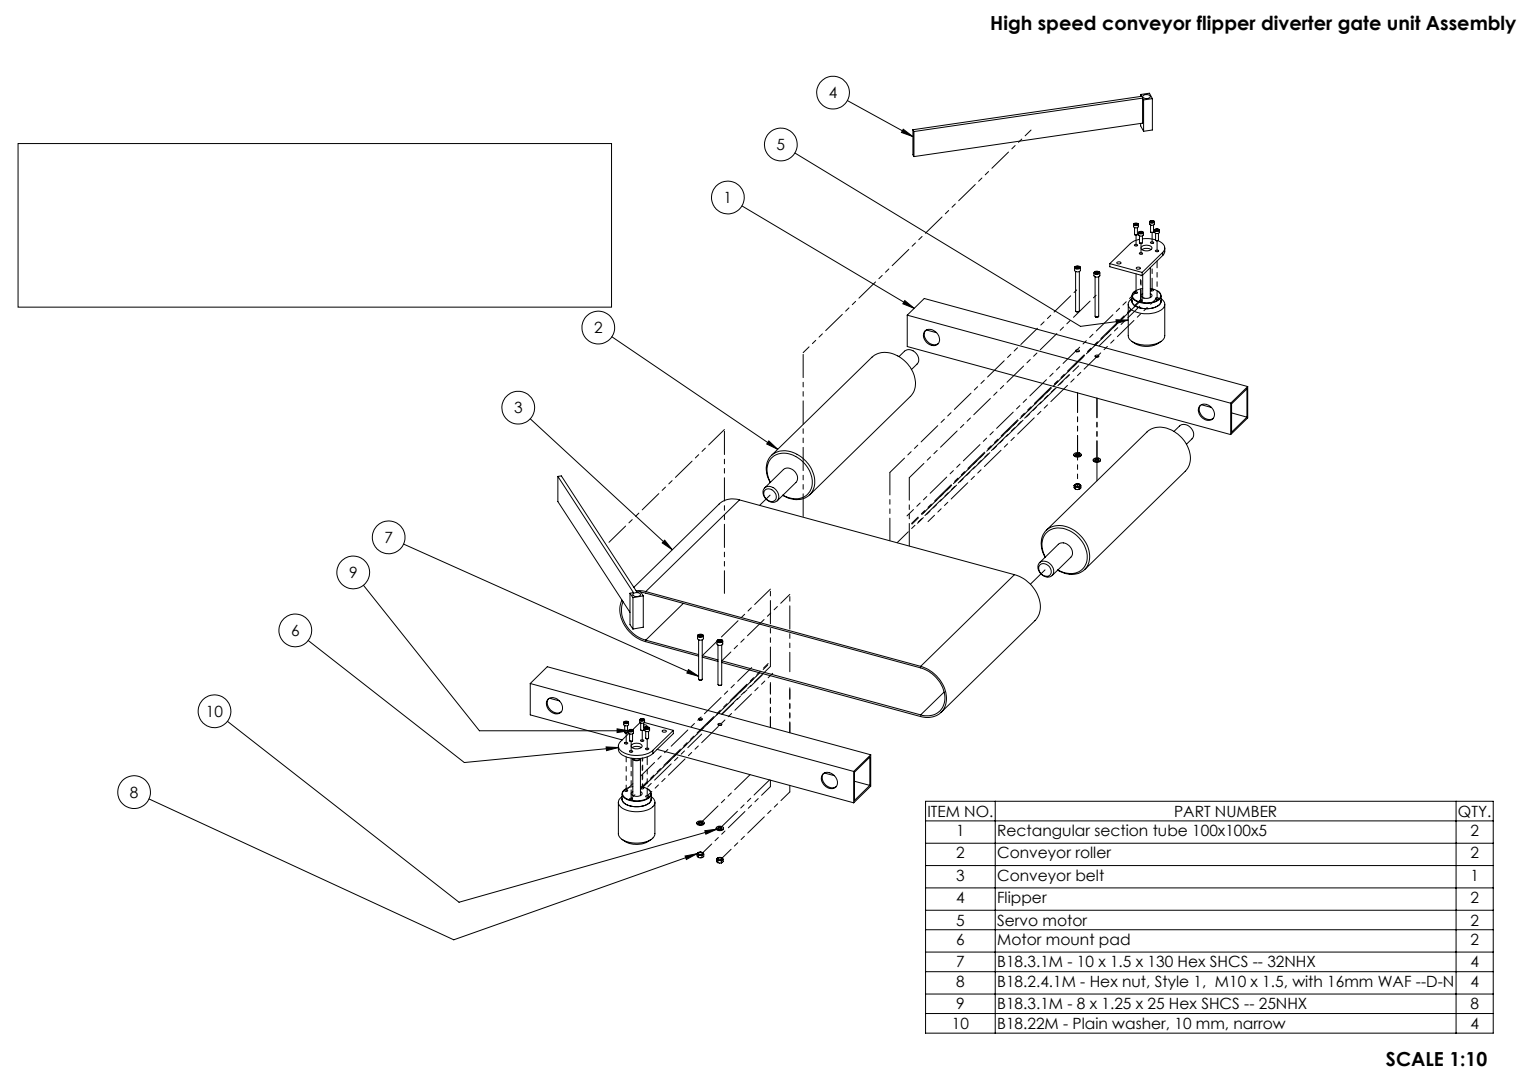
ISO-10303-21;
HEADER;
FILE_DESCRIPTION (('STEP AP214'),
    '1' );
FILE_NAME ('MAT-028',
    '2026-10-24T15:53:57',
    ( '' ),
    ( '' ),
    'SwSTEP 2.0',
    'SolidWorks 2025',
    '' );
FILE_SCHEMA (( 'AUTOMOTIVE_DESIGN' ));
ENDSEC;

DATA;
#1 = CARTESIAN_POINT ( 'NONE',  ( -86.99999999999945999, 120.0000000000003126, 10.00000000000000888 ) ) ;
#2 = DIRECTION ( 'NONE',  ( -3.851859888774471706E-33, -1.232595164407830946E-32, -1.000000000000000000 ) ) ;
#3 = FACE_BOUND ( 'NONE', #2659, .T. ) ;
#4 = FACE_BOUND ( 'NONE', #3829, .T. ) ;
#5 = VECTOR ( 'NONE', #7209, 1000.000000000000000 ) ;
#6 = CARTESIAN_POINT ( 'NONE',  ( -8.000000000000229150, -4.618802153516843312, -0.7145311798163467287 ) ) ;
#7 = EDGE_LOOP ( 'NONE', ( #379, #934, #6709, #4880 ) ) ;
#8 = FILL_AREA_STYLE ('',( #2739 ) ) ;
#9 = LINE ( 'NONE', #1201, #6141 ) ;
#10 = PRODUCT_RELATED_PRODUCT_CATEGORY ( 'part', '', ( #5732 ) ) ;
#11 = CARTESIAN_POINT ( 'NONE',  ( 8.000000000000229150, 4.618802153516954334, -8.400000000000018119 ) ) ;
#12 = CONICAL_SURFACE ( 'NONE', #4068, 9.499999999999998224, 0.7853981633974257415 ) ;
#13 = DIRECTION ( 'NONE',  ( -1.034996974062501909E-32, 0.7071067811865503483, 0.7071067811865446862 ) ) ;
#14 = DIRECTION ( 'NONE',  ( 0.000000000000000000, 0.000000000000000000, 1.000000000000000000 ) ) ;
#15 = CIRCLE ( 'NONE', #7701, 10.50000000000002132 ) ;
#16 = CARTESIAN_POINT ( 'NONE',  ( 3.319543390096325375, -7.321065037175607415, -8.383111142572088781 ) ) ;
#17 = CARTESIAN_POINT ( 'NONE',  ( -1.310872448938785073, 8.480771745766666925, -8.082649155111145234 ) ) ;
#18 = VERTEX_POINT ( 'NONE', #2644 ) ;
#19 = PLANE ( 'NONE',  #5290 ) ;
#20 = MANIFOLD_SOLID_BREP ( 'Cut-Extrude1', #1796 ) ;
#21 = VERTEX_POINT ( 'NONE', #2818 ) ;
#22 = CIRCLE ( 'NONE', #1145, 3.047499999999999876 ) ;
#23 = AXIS2_PLACEMENT_3D ( 'NONE', #7764, #3194, #2455 ) ;
#24 = CARTESIAN_POINT ( 'NONE',  ( 28.24999999999996092, 1.387778780781445676E-14, 18.00000000000000355 ) ) ;
#25 = ORIENTED_EDGE ( 'NONE', *, *, #2156, .F. ) ;
#26 = CYLINDRICAL_SURFACE ( 'NONE', #6690, 5.499999999999999112 ) ;
#27 = EDGE_CURVE ( 'NONE', #6851, #3192, #686, .T. ) ;
#28 = CARTESIAN_POINT ( 'NONE',  ( -0.6527133886630764881, 8.860760056385830197, -0.4969600502618033433 ) ) ;
#29 = DIRECTION ( 'NONE',  ( 8.659560562354951347E-17, 0.7071067811865459074, -0.7071067811865491270 ) ) ;
#30 = CIRCLE ( 'NONE', #2975, 8.000000000000007105 ) ;
#31 = DIRECTION ( 'NONE',  ( 1.000000000000000000, -3.549874073494553124E-30, -3.778304382545602261E-59 ) ) ;
#32 = CARTESIAN_POINT ( 'NONE',  ( 1.000000000000000888, 0.000000000000000000, 0.000000000000000000 ) ) ;
#33 = ORIENTED_EDGE ( 'NONE', *, *, #2623, .F. ) ;
#34 = CARTESIAN_POINT ( 'NONE',  ( -3.999999999999892530, 6.928203230275431501, -8.400000000000018119 ) ) ;
#35 = ORIENTED_EDGE ( 'NONE', *, *, #4431, .T. ) ;
#36 = VECTOR ( 'NONE', #1214, 1000.000000000000000 ) ;
#37 = PRODUCT_CONTEXT ( 'NONE', #2802, 'mechanical' ) ;
#38 = VECTOR ( 'NONE', #5500, 1000.000000000000000 ) ;
#39 = EDGE_CURVE ( 'NONE', #7000, #2703, #3383, .T. ) ;
#40 = MANIFOLD_SOLID_BREP ( 'EndChamfer', #8067 ) ;
#41 = CARTESIAN_POINT ( 'NONE',  ( 44.99999999999992895, -425.0000000000000000, -3.122502256758253953E-15 ) ) ;
#42 = ORIENTED_EDGE ( 'NONE', *, *, #2072, .T. ) ;
#43 = CARTESIAN_POINT ( 'NONE',  ( 15.00000000000000000, 1.836970198721029589E-15, -4.814824860968080875E-32 ) ) ;
#44 = CARTESIAN_POINT ( 'NONE',  ( -2.300000000000024247, 0.000000000000000000, 0.000000000000000000 ) ) ;
#45 = DIRECTION ( 'NONE',  ( 1.000000000000000000, 0.000000000000000000, 0.000000000000000000 ) ) ;
#46 = EDGE_LOOP ( 'NONE', ( #354, #6549, #4798, #4239, #7292 ) ) ;
#47 = EDGE_CURVE ( 'NONE', #2278, #2801, #888, .T. ) ;
#48 = EDGE_CURVE ( 'NONE', #6303, #1514, #1175, .T. ) ;
#49 = DIRECTION ( 'NONE',  ( 3.851859888774471706E-33, -7.598173571352223877E-18, 1.000000000000000000 ) ) ;
#50 = ORIENTED_EDGE ( 'NONE', *, *, #3725, .T. ) ;
#51 = PLANE ( 'NONE',  #3089 ) ;
#52 = ADVANCED_FACE ( 'NONE', ( #8577 ), #1878, .F. ) ;
#53 = CARTESIAN_POINT ( 'NONE',  ( 275.0000000000000000, -425.0000000000000000, 80.00000000000000000 ) ) ;
#54 = B_SPLINE_CURVE_WITH_KNOTS ( 'NONE', 3,
 ( #4820, #7477, #2036, #5217, #8413, #5353 ),
 .UNSPECIFIED., .F., .F.,
 ( 4, 2, 4 ),
 ( 0.008240550023493465118, 0.01057684187039403985, 0.01291313371729461458 ),
 .UNSPECIFIED. ) ;
#55 = CARTESIAN_POINT ( 'NONE',  ( -8.000000000000225597, 0.7809653281575857919, -1.307852751878529391E-13 ) ) ;
#56 = MANIFOLD_SOLID_BREP ( 'EndChamfer', #2646 ) ;
#57 = AXIS2_PLACEMENT_3D ( 'NONE', #6154, #7965, #2782 ) ;
#58 = DIRECTION ( 'NONE',  ( -3.851859888774471706E-33, 7.598173571352223877E-18, -1.000000000000000000 ) ) ;
#59 = DIRECTION ( 'NONE',  ( 3.919652622816902408E-30, 3.944304526105059027E-30, -1.000000000000000000 ) ) ;
#60 = ORIENTED_EDGE ( 'NONE', *, *, #341, .F. ) ;
#61 = CARTESIAN_POINT ( 'NONE',  ( 5.690023276062458280, 5.952467836904209442, -0.1306530452038583978 ) ) ;
#62 = ADVANCED_FACE ( 'NONE', ( #7235 ), #7793, .T. ) ;
#63 = PRODUCT_DEFINITION_SHAPE ( 'NONE', 'NONE',  #8606 ) ;
#64 = CARTESIAN_POINT ( 'NONE',  ( 5.354491962337593947, -6.146186931204438153, -8.331901280394781395 ) ) ;
#65 = LINE ( 'NONE', #1952, #3706 ) ;
#66 = CARTESIAN_POINT ( 'NONE',  ( 50.00000000000004263, 500.0000000000000000, -45.00000000000000711 ) ) ;
#67 = CARTESIAN_POINT ( 'NONE',  ( 4.000000000000003553, -6.928203230275542523, -8.400000000000018119 ) ) ;
#68 = ORIENTED_EDGE ( 'NONE', *, *, #5960, .T. ) ;
#69 = EDGE_CURVE ( 'NONE', #4173, #3196, #7937, .T. ) ;
#70 = CIRCLE ( 'NONE', #2861, 15.00000000000002487 ) ;
#71 = EDGE_LOOP ( 'NONE', ( #5393, #5239, #6082 ) ) ;
#72 = DIRECTION ( 'NONE',  ( -3.851859888774471706E-33, 7.598173571352223877E-18, -1.000000000000000000 ) ) ;
#73 = ORIENTED_EDGE ( 'NONE', *, *, #8357, .F. ) ;
#74 = CARTESIAN_POINT ( 'NONE',  ( -5.354491962338943090, 6.146186931204643322, -0.06809871960584383543 ) ) ;
#75 = DIRECTION ( 'NONE',  ( -3.919652622816902408E-30, -3.944304526105059027E-30, 1.000000000000000000 ) ) ;
#76 = CARTESIAN_POINT ( 'NONE',  ( 0.000000000000000000, 0.000000000000000000, -8.400000000000018119 ) ) ;
#77 = CARTESIAN_POINT ( 'NONE',  ( 8.000000000000007105, 0.000000000000000000, -8.400000000000018119 ) ) ;
#78 = ORIENTED_EDGE ( 'NONE', *, *, #1161, .F. ) ;
#79 = VERTEX_POINT ( 'NONE', #7978 ) ;
#80 = EDGE_CURVE ( 'NONE', #838, #2390, #1314, .T. ) ;
#81 = FACE_OUTER_BOUND ( 'NONE', #5518, .T. ) ;
#82 = DIRECTION ( 'NONE',  ( -1.463706757734299248E-32, 1.000000000000000000, 5.238529448733281520E-32 ) ) ;
#83 = SHAPE_REPRESENTATION ( 'socket head cap screw_am_B18.3.1M - 10 x 1.5 x 130 Hex SHCS -- 32NHX', ( #7563 ), #2282 ) ;
#84 = DIRECTION ( 'NONE',  ( 0.000000000000000000, 0.000000000000000000, 1.000000000000000000 ) ) ;
#85 = ORIENTED_EDGE ( 'NONE', *, *, #6307, .F. ) ;
#86 = CARTESIAN_POINT ( 'NONE',  ( 5.000000000000115463, -14.99999999999990230, 79.99999999999995737 ) ) ;
#87 = EDGE_CURVE ( 'NONE', #4142, #6381, #1356, .T. ) ;
#88 = VECTOR ( 'NONE', #1875, 1000.000000000000000 ) ;
#89 = DIRECTION ( 'NONE',  ( -1.000000000000000000, 0.000000000000000000, 0.000000000000000000 ) ) ;
#90 = ORIENTED_EDGE ( 'NONE', *, *, #5306, .F. ) ;
#91 = DIRECTION ( 'NONE',  ( -3.919652622816902408E-30, -3.944304526105059027E-30, 1.000000000000000000 ) ) ;
#92 = VERTEX_POINT ( 'NONE', #1262 ) ;
#93 = DIRECTION ( 'NONE',  ( 0.5000000000000035527, 0.8660254037844365982, 0.000000000000000000 ) ) ;
#94 = ORIENTED_EDGE ( 'NONE', *, *, #3041, .F. ) ;
#95 = FACE_BOUND ( 'NONE', #8531, .T. ) ;
#96 = DIRECTION ( 'NONE',  ( 0.000000000000000000, 0.000000000000000000, 1.000000000000000000 ) ) ;
#97 = CARTESIAN_POINT ( 'NONE',  ( 8.000000000000127898, -3.098204225878314233, -0.3157906771919719024 ) ) ;
#98 = EDGE_CURVE ( 'NONE', #113, #2214, #3687, .T. ) ;
#99 = CARTESIAN_POINT ( 'NONE',  ( -6.689127551062222565, -5.375634714784565560, -0.3173508448887311095 ) ) ;
#100 = ORIENTED_EDGE ( 'NONE', *, *, #87, .T. ) ;
#101 = DIRECTION ( 'NONE',  ( 1.000000000000000000, 8.881784197001244435E-16, 0.000000000000000000 ) ) ;
#102 = FILL_AREA_STYLE_COLOUR ( '', #7649 ) ;
#103 = CARTESIAN_POINT ( 'NONE',  ( -3.999999999999781508, -6.928203230275875590, 0.000000000000000000 ) ) ;
#104 =( REPRESENTATION_RELATIONSHIP ('NONE','NONE', #1279, #2397 ) REPRESENTATION_RELATIONSHIP_WITH_TRANSFORMATION ( #517 )SHAPE_REPRESENTATION_RELATIONSHIP( ) );
#105 = UNCERTAINTY_MEASURE_WITH_UNIT (LENGTH_MEASURE( 1.000000000000000082E-05 ), #1753, 'distance_accuracy_value', 'NONE');
#106 = AXIS2_PLACEMENT_3D ( 'NONE', #6926, #4870, #7530 ) ;
#107 = CARTESIAN_POINT ( 'NONE',  ( -2.300000000000024247, 0.000000000000000000, 0.000000000000000000 ) ) ;
#108 = EDGE_CURVE ( 'NONE', #7841, #5835, #6535, .T. ) ;
#109 = DIRECTION ( 'NONE',  ( 3.919652622816902408E-30, 3.944304526105059027E-30, -1.000000000000000000 ) ) ;
#110 = ITEM_DEFINED_TRANSFORMATION ( 'NONE', 'NONE', #1870,  #7563 ) ;
#111 = CARTESIAN_POINT ( 'NONE',  ( 2.309976723937863241, -7.903938623647072781, -8.269346954796054305 ) ) ;
#112 = CARTESIAN_POINT ( 'NONE',  ( 2.651878572103346281E-45, 7.470345474798193622E-16, 5.700000000000001954 ) ) ;
#113 = VERTEX_POINT ( 'NONE', #6673 ) ;
#114 = VECTOR ( 'NONE', #3316, 1000.000000000000000 ) ;
#115 = CIRCLE ( 'NONE', #6125, 4.250000000000013323 ) ;
#116 = CARTESIAN_POINT ( 'NONE',  ( 33.00000000000055422, -1.431146867680869324E-14, 3.309500000006883269 ) ) ;
#117 = ORIENTED_EDGE ( 'NONE', *, *, #6294, .F. ) ;
#118 = CARTESIAN_POINT ( 'NONE',  ( -6.661338147750939243E-13, -9.237604307034352757, -0.7145311798163467287 ) ) ;
#119 = CARTESIAN_POINT ( 'NONE',  ( 5.000000000000115463, -14.99999999999990230, 79.99999999999995737 ) ) ;
#120 = APPLICATION_CONTEXT ( 'automotive_design' ) ;
#121 = AXIS2_PLACEMENT_3D ( 'NONE', #7183, #2433, #3907 ) ;
#122 = LINE ( 'NONE', #2790, #5242 ) ;
#123 = AXIS2_PLACEMENT_3D ( 'NONE', #533, #8501, #5709 ) ;
#124 = ORIENTED_EDGE ( 'NONE', *, *, #2890, .F. ) ;
#125 = DIRECTION ( 'NONE',  ( 0.000000000000000000, -0.000000000000000000, 1.000000000000000000 ) ) ;
#126 = AXIS2_PLACEMENT_3D ( 'NONE', #3777, #2508, #508 ) ;
#127 = EDGE_LOOP ( 'NONE', ( #5459, #6206, #3231, #7547 ) ) ;
#128 = EDGE_LOOP ( 'NONE', ( #8016, #5711, #5284, #7956 ) ) ;
#129 = AXIS2_PLACEMENT_3D ( 'NONE', #5257, #6018, #4697 ) ;
#130 = DIRECTION ( 'NONE',  ( 0.000000000000000000, 0.000000000000000000, 1.000000000000000000 ) ) ;
#131 = AXIS2_PLACEMENT_3D ( 'NONE', #4497, #4378, #2324 ) ;
#132 = MANIFOLD_SOLID_BREP ( 'Cut-Extrude2', #7926 ) ;
#133 = EDGE_CURVE ( 'NONE', #2369, #4500, #873, .T. ) ;
#134 = AXIS2_PLACEMENT_3D ( 'NONE', #4752, #7312, #2784 ) ;
#135 = EDGE_LOOP ( 'NONE', ( #1045, #4350, #4597 ) ) ;
#136 = DIRECTION ( 'NONE',  ( -3.919652622816902408E-30, -3.944304526105059027E-30, 1.000000000000000000 ) ) ;
#137 = VECTOR ( 'NONE', #6845, 1000.000000000000000 ) ;
#138 = DIRECTION ( 'NONE',  ( 0.000000000000000000, -1.865174681370262041E-14, -1.000000000000000000 ) ) ;
#139 = DIRECTION ( 'NONE',  ( 0.000000000000000000, 0.000000000000000000, 1.000000000000000000 ) ) ;
#140 = ORIENTED_EDGE ( 'NONE', *, *, #515, .T. ) ;
#141 = VECTOR ( 'NONE', #1678, 1000.000000000000000 ) ;
#142 = ORIENTED_EDGE ( 'NONE', *, *, #672, .F. ) ;
#143 = DIRECTION ( 'NONE',  ( 0.000000000000000000, 0.000000000000000000, 1.000000000000000000 ) ) ;
#144 = EDGE_CURVE ( 'NONE', #3620, #2938, #3568, .T. ) ;
#145 = FACE_OUTER_BOUND ( 'NONE', #4016, .T. ) ;
#146 = ORIENTED_EDGE ( 'NONE', *, *, #4273, .F. ) ;
#147 = DIRECTION ( 'NONE',  ( 1.000000000000000000, 0.000000000000000000, 0.000000000000000000 ) ) ;
#148 = CARTESIAN_POINT ( 'NONE',  ( 5.000000000000004441, 2.342598717236861638, 4.057500000000047180 ) ) ;
#149 = EDGE_LOOP ( 'NONE', ( #8051, #8502, #8444, #3963, #8407 ) ) ;
#150 =( NAMED_UNIT ( * ) PLANE_ANGLE_UNIT ( ) SI_UNIT ( $, .RADIAN. ) );
#151 = CARTESIAN_POINT ( 'NONE',  ( 39.75000000000007105, 4.867971026610737916E-15, 18.00000000000000355 ) ) ;
#152 = CARTESIAN_POINT ( 'NONE',  ( -5.690023276062281532, -5.952467836904624221, -0.1306530452039605383 ) ) ;
#153 = EDGE_CURVE ( 'NONE', #8158, #6208, #162, .T. ) ;
#154 = ADVANCED_FACE ( 'NONE', ( #2295 ), #1559, .T. ) ;
#155 = DIRECTION ( 'NONE',  ( 0.000000000000000000, 0.000000000000000000, 1.000000000000000000 ) ) ;
#156 = CARTESIAN_POINT ( 'NONE',  ( 3.999999999999337419, -6.928203230275431501, 0.000000000000000000 ) ) ;
#157 = CYLINDRICAL_SURFACE ( 'NONE', #5418, 80.00000000000000000 ) ;
#158 = DIRECTION ( 'NONE',  ( 1.463706757734299248E-32, -1.000000000000000000, -5.238529448733281520E-32 ) ) ;
#159 = ORIENTED_EDGE ( 'NONE', *, *, #1330, .T. ) ;
#160 = CARTESIAN_POINT ( 'NONE',  ( -8.000000000000666134, -3.867591403078895596, -0.4976753153248583139 ) ) ;
#161 = ORIENTED_EDGE ( 'NONE', *, *, #1345, .T. ) ;
#162 = CIRCLE ( 'NONE', #5164, 5.700000000000001954 ) ;
#163 = DIRECTION ( 'NONE',  ( -1.000000000000000000, 0.000000000000000000, 6.938893903907228378E-17 ) ) ;
#164 = AXIS2_PLACEMENT_3D ( 'NONE', #7493, #6114, #5025 ) ;
#165 = EDGE_CURVE ( 'NONE', #2264, #3370, #4990, .T. ) ;
#166 =( NAMED_UNIT ( * ) SI_UNIT ( $, .STERADIAN. ) SOLID_ANGLE_UNIT ( ) );
#167 = CARTESIAN_POINT ( 'NONE',  ( -99.99999999999961631, 120.0000000000001137, 10.00000000000000888 ) ) ;
#168 = AXIS2_PLACEMENT_3D ( 'NONE', #382, #5715, #8345 ) ;
#169 = DIRECTION ( 'NONE',  ( -3.851859888774471706E-33, -1.232595164407830946E-32, -1.000000000000000000 ) ) ;
#170 = EDGE_LOOP ( 'NONE', ( #1899, #7245, #7698, #4667, #2525, #5079 ) ) ;
#171 = VECTOR ( 'NONE', #3121, 999.9999999999998863 ) ;
#172 = DIRECTION ( 'NONE',  ( -0.000000000000000000, -0.000000000000000000, 1.000000000000000000 ) ) ;
#173 = VERTEX_POINT ( 'NONE', #4952 ) ;
#174 = VECTOR ( 'NONE', #663, 1000.000000000000000 ) ;
#175 = ORIENTED_EDGE ( 'NONE', *, *, #1489, .T. ) ;
#176 = AXIS2_PLACEMENT_3D ( 'NONE', #7035, #983, #7228 ) ;
#177 = EDGE_CURVE ( 'NONE', #5857, #5352, #6924, .T. ) ;
#178 = VECTOR ( 'NONE', #4210, 1000.000000000000000 ) ;
#179 = CARTESIAN_POINT ( 'NONE',  ( 0.000000000000000000, 0.000000000000000000, -50.00000000000000000 ) ) ;
#180 = AXIS2_PLACEMENT_3D ( 'NONE', #8116, #8071, #4145 ) ;
#181 = VERTEX_POINT ( 'NONE', #3609 ) ;
#182 = CARTESIAN_POINT ( 'NONE',  ( 10.00000000000012079, -29.14213562373080180, 0.000000000000000000 ) ) ;
#183 = CIRCLE ( 'NONE', #891, 19.49999999999996803 ) ;
#184 = CARTESIAN_POINT ( 'NONE',  ( 350.0000000000001137, 59.99999999999887024, 69.99999999999995737 ) ) ;
#185 = ORIENTED_EDGE ( 'NONE', *, *, #1131, .T. ) ;
#186 = DIRECTION ( 'NONE',  ( 1.000000000000000000, 0.000000000000000000, 0.000000000000000000 ) ) ;
#187 = ORIENTED_EDGE ( 'NONE', *, *, #8140, .F. ) ;
#188 = DIRECTION ( 'NONE',  ( -0.8660254037844362651, -0.5000000000000039968, 0.000000000000000000 ) ) ;
#189 = AXIS2_PLACEMENT_3D ( 'NONE', #4605, #682, #3336 ) ;
#190 = CARTESIAN_POINT ( 'NONE',  ( 0.000000000000000000, 9.237604307034130713, -7.685468820183672278 ) ) ;
#191 = ORIENTED_EDGE ( 'NONE', *, *, #5664, .F. ) ;
#192 = DIRECTION ( 'NONE',  ( -1.000000000000000000, -8.881784197001244435E-16, -0.000000000000000000 ) ) ;
#193 = CARTESIAN_POINT ( 'NONE',  ( 8.000000000000229150, -1.665334536937734811E-13, 0.000000000000000000 ) ) ;
#194 = CARTESIAN_POINT ( 'NONE',  ( -34.92499999999998295, 0.000000000000000000, 0.000000000000000000 ) ) ;
#195 =( NAMED_UNIT ( * ) SI_UNIT ( $, .STERADIAN. ) SOLID_ANGLE_UNIT ( ) );
#196 = ORIENTED_EDGE ( 'NONE', *, *, #805, .T. ) ;
#197 = ADVANCED_FACE ( 'NONE', ( #1042 ), #6035, .F. ) ;
#198 = ORIENTED_EDGE ( 'NONE', *, *, #1594, .T. ) ;
#199 =( GEOMETRIC_REPRESENTATION_CONTEXT ( 3 ) GLOBAL_UNCERTAINTY_ASSIGNED_CONTEXT ( ( #3695 ) ) GLOBAL_UNIT_ASSIGNED_CONTEXT ( ( #528, #3762, #1023 ) ) REPRESENTATION_CONTEXT ( 'NONE', 'WORKASPACE' ) );
#200 = CARTESIAN_POINT ( 'NONE',  ( 6.686525924292749501, -5.377136764700527927, -8.083279549040062406 ) ) ;
#201 = CIRCLE ( 'NONE', #4665, 25.00000000000000711 ) ;
#202 = CARTESIAN_POINT ( 'NONE',  ( 1.310872448937509205, -8.480771745766409353, -0.3173508448886196431 ) ) ;
#203 = CARTESIAN_POINT ( 'NONE',  ( 5.000000000000115463, 7.027796151710889561, -4.057500000000047180 ) ) ;
#204 = DIRECTION ( 'NONE',  ( 1.000000000000000000, -3.549874073494553124E-30, 0.000000000000000000 ) ) ;
#205 = CONICAL_SURFACE ( 'NONE', #4669, 8.000000000000007105, 1.047197551196597631 ) ;
#206 = CARTESIAN_POINT ( 'NONE',  ( -50.00000000000004263, 425.0000000000000000, 25.00000000000001066 ) ) ;
#207 = EDGE_LOOP ( 'NONE', ( #1622, #7247, #78 ) ) ;
#208 = EDGE_CURVE ( 'NONE', #8055, #316, #7571, .T. ) ;
#209 = CARTESIAN_POINT ( 'NONE',  ( 10.00000000000000888, 8.000000000000001776, 4.440892098500626162E-13 ) ) ;
#210 = ORIENTED_EDGE ( 'NONE', *, *, #6998, .T. ) ;
#211 = CARTESIAN_POINT ( 'NONE',  ( -275.0000000000000000, -425.0000000000000000, 75.00000000000000000 ) ) ;
#212 = ADVANCED_BREP_SHAPE_REPRESENTATION ( '', ( #5685, #7563 ), #1720 ) ;
#213 = CYLINDRICAL_SURFACE ( 'NONE', #3938, 5.000000000000034639 ) ;
#214 = ORIENTED_EDGE ( 'NONE', *, *, #1634, .F. ) ;
#215 = CARTESIAN_POINT ( 'NONE',  ( -7.999999999999785061, 4.618802153516954334, -7.685468820183672278 ) ) ;
#216 = ORIENTED_EDGE ( 'NONE', *, *, #7702, .T. ) ;
#217 = VECTOR ( 'NONE', #7393, 1000.000000000000000 ) ;
#218 = VERTEX_POINT ( 'NONE', #2995 ) ;
#219 = EDGE_CURVE ( 'NONE', #4124, #477, #2955, .T. ) ;
#220 = DIRECTION ( 'NONE',  ( -1.774937036747276562E-30, -1.000000000000000000, -5.322451846059955323E-30 ) ) ;
#221 = AXIS2_PLACEMENT_3D ( 'NONE', #2814, #2077, #2895 ) ;
#222 = EDGE_CURVE ( 'NONE', #7027, #6175, #4345, .T. ) ;
#223 = CARTESIAN_POINT ( 'NONE',  ( 0.000000000000000000, 0.000000000000000000, -8.401000000000047763 ) ) ;
#224 = ORIENTED_EDGE ( 'NONE', *, *, #6569, .F. ) ;
#225 = CARTESIAN_POINT ( 'NONE',  ( 5.000000000000115463, 7.027796151710889561, -4.057500000000047180 ) ) ;
#226 = VECTOR ( 'NONE', #5474, 1000.000000000000000 ) ;
#227 = DIRECTION ( 'NONE',  ( -3.851859888774471706E-33, 7.598173571352223877E-18, -1.000000000000000000 ) ) ;
#228 = DIRECTION ( 'NONE',  ( 1.665334536937733578E-16, 1.000000000000000222, 8.736544766236841892E-16 ) ) ;
#229 = ORIENTED_EDGE ( 'NONE', *, *, #2672, .F. ) ;
#230 = ADVANCED_BREP_SHAPE_REPRESENTATION ( '', ( #2980, #7563 ), #1574 ) ;
#231 = CARTESIAN_POINT ( 'NONE',  ( 5.000000000000115463, -14.99999999999990230, -20.00100000000004741 ) ) ;
#232 = VERTEX_POINT ( 'NONE', #290 ) ;
#233 = CARTESIAN_POINT ( 'NONE',  ( -5.080504117408889186, -2.106769544347818268, -8.400000000000018119 ) ) ;
#234 = DIRECTION ( 'NONE',  ( 1.000000000000000000, 0.000000000000000000, 0.000000000000000000 ) ) ;
#235 = LINE ( 'NONE', #7430, #3287 ) ;
#236 = EDGE_LOOP ( 'NONE', ( #4101, #6935, #4324 ) ) ;
#237 = DIRECTION ( 'NONE',  ( -3.919652622816902408E-30, -3.944304526105059027E-30, 1.000000000000000000 ) ) ;
#238 = FACE_BOUND ( 'NONE', #6984, .T. ) ;
#239 = ORIENTED_EDGE ( 'NONE', *, *, #4179, .F. ) ;
#240 = ORIENTED_EDGE ( 'NONE', *, *, #8498, .T. ) ;
#241 = DIRECTION ( 'NONE',  ( 3.851859888774471706E-33, -7.598173571352223877E-18, 1.000000000000000000 ) ) ;
#242 = VECTOR ( 'NONE', #7821, 1000.000000000000000 ) ;
#243 = CARTESIAN_POINT ( 'NONE',  ( 0.000000000000000000, 0.000000000000000000, -8.400000000000018119 ) ) ;
#244 = PLANE ( 'NONE',  #5375 ) ;
#245 = EDGE_CURVE ( 'NONE', #3380, #4181, #3653, .T. ) ;
#246 = CARTESIAN_POINT ( 'NONE',  ( -86.99999999999944578, 120.0000000000003126, 10.00000000000000888 ) ) ;
#247 = CARTESIAN_POINT ( 'NONE',  ( 8.000000000000229150, -4.440892098500626162E-13, 0.000000000000000000 ) ) ;
#248 = ORIENTED_EDGE ( 'NONE', *, *, #4056, .T. ) ;
#249 = CARTESIAN_POINT ( 'NONE',  ( 5.551115123125782702E-14, 3.518949890710790118, 2.220446049250313081E-13 ) ) ;
#250 = ORIENTED_EDGE ( 'NONE', *, *, #1425, .T. ) ;
#251 = DIRECTION ( 'NONE',  ( 0.000000000000000000, -1.213383262747659708E-29, 1.000000000000000000 ) ) ;
#252 = DIRECTION ( 'NONE',  ( -7.420547859534711256E-34, 1.000000000000000000, 1.224646799147352961E-16 ) ) ;
#253 = DIRECTION ( 'NONE',  ( -7.703719777548943412E-34, 0.000000000000000000, 1.000000000000000000 ) ) ;
#254 = EDGE_CURVE ( 'NONE', #4707, #18, #5614, .T. ) ;
#255 = ORIENTED_EDGE ( 'NONE', *, *, #2015, .T. ) ;
#256 = DIRECTION ( 'NONE',  ( -7.420547859534711256E-34, 1.000000000000000000, 1.224646799147352961E-16 ) ) ;
#257 = ORIENTED_EDGE ( 'NONE', *, *, #5557, .F. ) ;
#258 = ORIENTED_EDGE ( 'NONE', *, *, #80, .F. ) ;
#259 = CIRCLE ( 'NONE', #4435, 3.047499999999999876 ) ;
#260 = CARTESIAN_POINT ( 'NONE',  ( 0.000000000000000000, -2.342598717236902939, 4.057500000000047180 ) ) ;
#261 = DIRECTION ( 'NONE',  ( 0.000000000000000000, -1.000000000000000000, -1.224646799147352714E-16 ) ) ;
#262 = ADVANCED_FACE ( 'NONE', ( #7614 ), #6970, .T. ) ;
#263 = FACE_OUTER_BOUND ( 'NONE', #2610, .T. ) ;
#264 = ORIENTED_EDGE ( 'NONE', *, *, #6676, .F. ) ;
#265 = AXIS2_PLACEMENT_3D ( 'NONE', #591, #6694, #3898 ) ;
#266 = CONICAL_SURFACE ( 'NONE', #4861, 4.171999999999999709, 0.7853981633975604115 ) ;
#267 = DIRECTION ( 'NONE',  ( 1.000000000000000000, 0.000000000000000000, -0.000000000000000000 ) ) ;
#268 = CONICAL_SURFACE ( 'NONE', #8331, 8.000000000000007105, 1.047197551196597631 ) ;
#269 = DIRECTION ( 'NONE',  ( -4.579669976578770729E-16, -5.898059818321084956E-17, -1.000000000000000000 ) ) ;
#270 = EDGE_LOOP ( 'NONE', ( #1206, #6558, #6515, #500 ) ) ;
#271 = AXIS2_PLACEMENT_3D ( 'NONE', #6647, #2, #2074 ) ;
#272 = DIRECTION ( 'NONE',  ( -0.000000000000000000, -0.000000000000000000, 1.000000000000000000 ) ) ;
#273 = CIRCLE ( 'NONE', #8348, 6.500000000000000888 ) ;
#274 = CIRCLE ( 'NONE', #551, 8.000000000000007105 ) ;
#275 = ORIENTED_EDGE ( 'NONE', *, *, #2858, .F. ) ;
#276 = DIRECTION ( 'NONE',  ( 3.549874073494553124E-30, 1.000000000000000000, -1.224646799147246711E-16 ) ) ;
#277 = ADVANCED_FACE ( 'NONE', ( #3520 ), #6195, .F. ) ;
#278 = CIRCLE ( 'NONE', #4737, 38.74999999999999289 ) ;
#279 = AXIS2_PLACEMENT_3D ( 'NONE', #7241, #6496, #6681 ) ;
#280 = AXIS2_PLACEMENT_3D ( 'NONE', #7220, #2059, #7465 ) ;
#281 = DIRECTION ( 'NONE',  ( 0.000000000000000000, 0.000000000000000000, -1.000000000000000000 ) ) ;
#282 = VERTEX_POINT ( 'NONE', #3737 ) ;
#283 = DIRECTION ( 'NONE',  ( 1.000000000000000000, 0.000000000000000000, 0.000000000000000000 ) ) ;
#284 = ORIENTED_EDGE ( 'NONE', *, *, #3202, .F. ) ;
#285 =( GEOMETRIC_REPRESENTATION_CONTEXT ( 3 ) GLOBAL_UNCERTAINTY_ASSIGNED_CONTEXT ( ( #4742 ) ) GLOBAL_UNIT_ASSIGNED_CONTEXT ( ( #5304, #150, #6149 ) ) REPRESENTATION_CONTEXT ( 'NONE', 'WORKASPACE' ) );
#286 = EDGE_LOOP ( 'NONE', ( #851, #3513, #5956 ) ) ;
#287 = AXIS2_PLACEMENT_3D ( 'NONE', #7730, #8435, #429 ) ;
#288 = DIRECTION ( 'NONE',  ( 0.000000000000000000, 0.000000000000000000, 1.000000000000000000 ) ) ;
#289 = CARTESIAN_POINT ( 'NONE',  ( 0.000000000000000000, 0.000000000000000000, -8.400000000000018119 ) ) ;
#290 = CARTESIAN_POINT ( 'NONE',  ( 4.000000000000003553, 1.759474945355374409, 3.047499999999869758 ) ) ;
#291 = DIRECTION ( 'NONE',  ( 0.000000000000000000, -5.322451846059955323E-30, 1.000000000000000000 ) ) ;
#292 = DIRECTION ( 'NONE',  ( 1.000000000000000000, 2.715219353702832714E-15, 0.000000000000000000 ) ) ;
#293 = ORIENTED_EDGE ( 'NONE', *, *, #7605, .F. ) ;
#294 = CARTESIAN_POINT ( 'NONE',  ( -6.661338147750939243E-13, -9.237604307034352757, -0.7145311798163467287 ) ) ;
#295 = ORIENTED_EDGE ( 'NONE', *, *, #7376, .F. ) ;
#296 = EDGE_CURVE ( 'NONE', #662, #1055, #1974, .T. ) ;
#297 = PRODUCT_DEFINITION ( 'UNKNOWN', '', #2849, #7006 ) ;
#298 =( LENGTH_UNIT ( ) NAMED_UNIT ( * ) SI_UNIT ( .MILLI., .METRE. ) );
#299 = LINE ( 'NONE', #1008, #2699 ) ;
#300 = ORIENTED_EDGE ( 'NONE', *, *, #47, .F. ) ;
#301 = CYLINDRICAL_SURFACE ( 'NONE', #1407, 6.500000000000001776 ) ;
#302 = ORIENTED_EDGE ( 'NONE', *, *, #1070, .T. ) ;
#303 = VERTEX_POINT ( 'NONE', #1894 ) ;
#304 = VECTOR ( 'NONE', #6582, 1000.000000000000114 ) ;
#305 = VECTOR ( 'NONE', #380, 1000.000000000000000 ) ;
#306 = EDGE_CURVE ( 'NONE', #6636, #757, #6561, .T. ) ;
#307 = CARTESIAN_POINT ( 'NONE',  ( 1.000000000000000888, -4.257961476847964819E-29, 8.000000000000001776 ) ) ;
#308 = AXIS2_PLACEMENT_3D ( 'NONE', #203, #4215, #7047 ) ;
#309 = CARTESIAN_POINT ( 'NONE',  ( 3.000384657911014680E-15, -299.9999999999999432, -24.50000000000001776 ) ) ;
#310 = DIRECTION ( 'NONE',  ( 0.000000000000000000, 5.322451846059955323E-30, -1.000000000000000000 ) ) ;
#311 = EDGE_LOOP ( 'NONE', ( #3317, #6178 ) ) ;
#312 = AXIS2_PLACEMENT_3D ( 'NONE', #6347, #6261, #6422 ) ;
#313 = CARTESIAN_POINT ( 'NONE',  ( -9.999999999999884537, -14.99999999999990052, -20.00000000000001776 ) ) ;
#314 = CARTESIAN_POINT ( 'NONE',  ( -8.000000000000001776, 0.7809653281576423023, -8.400000000000011013 ) ) ;
#315 = CARTESIAN_POINT ( 'NONE',  ( 455.0000000000001137, 29.99999999999980460, 31.99999999999993250 ) ) ;
#316 = VERTEX_POINT ( 'NONE', #7169 ) ;
#317 = DIRECTION ( 'NONE',  ( -1.000000000000000000, 0.000000000000000000, 0.000000000000000000 ) ) ;
#318 = ADVANCED_FACE ( 'NONE', ( #509 ), #5075, .F. ) ;
#319 = VECTOR ( 'NONE', #7151, 1000.000000000000000 ) ;
#320 = AXIS2_PLACEMENT_3D ( 'NONE', #2121, #5234, #1317 ) ;
#321 = ORIENTED_EDGE ( 'NONE', *, *, #108, .F. ) ;
#322 = CARTESIAN_POINT ( 'NONE',  ( -6.661338147750939243E-13, 9.237604307034352757, -0.7145311798163467287 ) ) ;
#323 = DIRECTION ( 'NONE',  ( 1.463706757734299248E-32, -1.000000000000000000, -5.238529448733281520E-32 ) ) ;
#324 = DIRECTION ( 'NONE',  ( 1.000000000000000000, 0.000000000000000000, 0.000000000000000000 ) ) ;
#325 = EDGE_LOOP ( 'NONE', ( #1288, #5702, #5068, #5725 ) ) ;
#326 = AXIS2_PLACEMENT_3D ( 'NONE', #7150, #8255, #3831 ) ;
#327 = B_SPLINE_CURVE_WITH_KNOTS ( 'NONE', 3,
 ( #6752, #6150, #2862, #1472, #6922, #4786, #4128, #948 ),
 .UNSPECIFIED., .F., .F.,
 ( 4, 2, 2, 4 ),
 ( 0.004673709593152389034, 0.005837709341827845497, 0.007001709090503301092, 0.009329708587854212282 ),
 .UNSPECIFIED. ) ;
#328 = DIRECTION ( 'NONE',  ( 3.919652622816902408E-30, 3.944304526105059027E-30, -1.000000000000000000 ) ) ;
#329 = ORIENTED_EDGE ( 'NONE', *, *, #2161, .T. ) ;
#330 = CIRCLE ( 'NONE', #8396, 5.500000000000000000 ) ;
#331 = AXIS2_PLACEMENT_3D ( 'NONE', #1287, #6747, #4081 ) ;
#332 = ADVANCED_FACE ( 'NONE', ( #3201 ), #4425, .F. ) ;
#333 = ORIENTED_EDGE ( 'NONE', *, *, #4840, .F. ) ;
#334 = CARTESIAN_POINT ( 'NONE',  ( -31.74999999999994316, -6.918267515436165433E-29, 6.500000000000001776 ) ) ;
#335 = EDGE_CURVE ( 'NONE', #2009, #7164, #7911, .T. ) ;
#336 = AXIS2_PLACEMENT_3D ( 'NONE', #6289, #351, #5640 ) ;
#337 = CARTESIAN_POINT ( 'NONE',  ( 0.000000000000000000, 0.000000000000000000, 10.00000000000000888 ) ) ;
#338 = FACE_OUTER_BOUND ( 'NONE', #5605, .T. ) ;
#339 = AXIS2_PLACEMENT_3D ( 'NONE', #8203, #2233, #4890 ) ;
#340 = CARTESIAN_POINT ( 'NONE',  ( 5.000000000000115463, -14.99999999999990230, -20.00000000000001776 ) ) ;
#341 = EDGE_CURVE ( 'NONE', #5769, #3947, #5762, .T. ) ;
#342 = DIRECTION ( 'NONE',  ( -1.000000000000000000, -8.881784197001244435E-16, 0.000000000000000000 ) ) ;
#343 = EDGE_CURVE ( 'NONE', #1391, #6892, #2509, .T. ) ;
#344 = DIRECTION ( 'NONE',  ( -1.463706757734299248E-32, 1.000000000000000000, 5.238529448733281520E-32 ) ) ;
#345 = DIRECTION ( 'NONE',  ( 0.000000000000000000, 0.000000000000000000, 1.000000000000000000 ) ) ;
#346 = CARTESIAN_POINT ( 'NONE',  ( 10.40000000000001990, 0.000000000000000000, 4.440892098500626162E-13 ) ) ;
#347 = EDGE_LOOP ( 'NONE', ( #894, #7668, #7763, #5691 ) ) ;
#348 = DIRECTION ( 'NONE',  ( 0.8660254037844369313, 0.5000000000000028866, 0.000000000000000000 ) ) ;
#349 = EDGE_LOOP ( 'NONE', ( #8567, #7079, #5619, #6305, #3841, #1034 ) ) ;
#350 = PRODUCT_DEFINITION_FORMATION_WITH_SPECIFIED_SOURCE ( 'ANY', '', #5732, .NOT_KNOWN. ) ;
#351 = DIRECTION ( 'NONE',  ( -3.919652622816902408E-30, -3.944304526105059027E-30, 1.000000000000000000 ) ) ;
#352 = DIRECTION ( 'NONE',  ( -0.7071067811865456854, -8.706684567168461317E-33, -0.7071067811865493491 ) ) ;
#353 = ORIENTED_EDGE ( 'NONE', *, *, #7620, .T. ) ;
#354 = ORIENTED_EDGE ( 'NONE', *, *, #6370, .T. ) ;
#355 = CIRCLE ( 'NONE', #3273, 5.559999999999998721 ) ;
#356 = VECTOR ( 'NONE', #2554, 1000.000000000000000 ) ;
#357 = UNCERTAINTY_MEASURE_WITH_UNIT (LENGTH_MEASURE( 1.000000000000000082E-05 ), #6514, 'distance_accuracy_value', 'NONE');
#358 = DIRECTION ( 'NONE',  ( -1.000000000000000000, 0.000000000000000000, 0.000000000000000000 ) ) ;
#359 = VECTOR ( 'NONE', #6067, 1000.000000000000000 ) ;
#360 = CARTESIAN_POINT ( 'NONE',  ( 44.99999999999992895, -425.0000000000000000, 25.00000000000000355 ) ) ;
#361 = CARTESIAN_POINT ( 'NONE',  ( 1.110223024625156540E-13, 9.237604307033992157, -8.400000000000018119 ) ) ;
#362 = ADVANCED_FACE ( 'NONE', ( #2551 ), #3698, .F. ) ;
#363 = VERTEX_POINT ( 'NONE', #3075 ) ;
#364 = DIRECTION ( 'NONE',  ( -6.400024471207001551E-36, 1.000000000000000000, 7.598173571352213092E-18 ) ) ;
#365 = CARTESIAN_POINT ( 'NONE',  ( -99.99999999999972999, 0.000000000000000000, 9.999999999999980460 ) ) ;
#366 = SHAPE_DEFINITION_REPRESENTATION ( #7163, #2397 ) ;
#367 = VERTEX_POINT ( 'NONE', #1117 ) ;
#368 = CYLINDRICAL_SURFACE ( 'NONE', #7232, 10.49999999999999645 ) ;
#369 = VERTEX_POINT ( 'NONE', #3034 ) ;
#370 = CARTESIAN_POINT ( 'NONE',  ( 1.521569672518448540E-45, 8.572527594031101439E-16, 7.000000000000000888 ) ) ;
#371 = CARTESIAN_POINT ( 'NONE',  ( 0.000000000000000000, 0.000000000000000000, -8.400000000000018119 ) ) ;
#372 = ADVANCED_FACE ( 'NONE', ( #5721 ), #1722, .F. ) ;
#373 = ORIENTED_EDGE ( 'NONE', *, *, #1689, .F. ) ;
#374 = CONICAL_SURFACE ( 'NONE', #5238, 8.000000000000007105, 1.047197551196597631 ) ;
#375 = CARTESIAN_POINT ( 'NONE',  ( 8.000000000000229150, -1.665334536937734811E-13, -8.400000000000018119 ) ) ;
#376 =( NAMED_UNIT ( * ) PLANE_ANGLE_UNIT ( ) SI_UNIT ( $, .RADIAN. ) );
#377 = ORIENTED_EDGE ( 'NONE', *, *, #1254, .F. ) ;
#378 = CARTESIAN_POINT ( 'NONE',  ( 44.99999999999992895, 500.0000000000000000, 45.00000000000000711 ) ) ;
#379 = ORIENTED_EDGE ( 'NONE', *, *, #5089, .T. ) ;
#380 = DIRECTION ( 'NONE',  ( -1.619075244245011540E-15, -1.000000000000000000, 3.747089299799789961E-30 ) ) ;
#381 = ORIENTED_EDGE ( 'NONE', *, *, #1415, .T. ) ;
#382 = CARTESIAN_POINT ( 'NONE',  ( 0.000000000000000000, 0.000000000000000000, -8.400000000000018119 ) ) ;
#383 = AXIS2_PLACEMENT_3D ( 'NONE', #3939, #7208, #1372 ) ;
#384 = CIRCLE ( 'NONE', #8575, 25.00000000000000711 ) ;
#385 = CARTESIAN_POINT ( 'NONE',  ( 0.000000000000000000, 0.000000000000000000, -8.401000000000047763 ) ) ;
#386 = EDGE_CURVE ( 'NONE', #7541, #369, #1275, .T. ) ;
#387 = DIRECTION ( 'NONE',  ( 0.000000000000000000, 0.000000000000000000, 1.000000000000000000 ) ) ;
#388 = CARTESIAN_POINT ( 'NONE',  ( -4.000000000000114575, -6.928203230275542523, -8.400000000000018119 ) ) ;
#389 = DIRECTION ( 'NONE',  ( 0.000000000000000000, 0.000000000000000000, 1.000000000000000000 ) ) ;
#390 = ORIENTED_EDGE ( 'NONE', *, *, #2485, .F. ) ;
#391 = EDGE_CURVE ( 'NONE', #8158, #7966, #6399, .T. ) ;
#392 = FACE_OUTER_BOUND ( 'NONE', #493, .T. ) ;
#393 = ORIENTED_EDGE ( 'NONE', *, *, #1927, .F. ) ;
#394 = EDGE_CURVE ( 'NONE', #7471, #7660, #2461, .T. ) ;
#395 = CARTESIAN_POINT ( 'NONE',  ( 8.000000000000012434, 0.7809653281576667272, -8.400000000000012790 ) ) ;
#396 = CONTEXT_DEPENDENT_SHAPE_REPRESENTATION ( #7407, #5586 ) ;
#397 = DIRECTION ( 'NONE',  ( -3.851859888774471706E-33, -1.232595164407830946E-32, -1.000000000000000000 ) ) ;
#398 = VECTOR ( 'NONE', #4921, 1000.000000000000000 ) ;
#399 = ORIENTED_EDGE ( 'NONE', *, *, #5241, .T. ) ;
#400 = CARTESIAN_POINT ( 'NONE',  ( 4.000000000000114575, 6.928203230275597591, -8.400000000000018119 ) ) ;
#401 = B_SPLINE_CURVE_WITH_KNOTS ( 'NONE', 3,
 ( #1259, #743, #8059, #702, #2750, #2709 ),
 .UNSPECIFIED., .F., .F.,
 ( 4, 2, 4 ),
 ( 0.008240550023493506751, 0.01057684187039422546, 0.01291313371729494418 ),
 .UNSPECIFIED. ) ;
#402 = EDGE_CURVE ( 'NONE', #7042, #3286, #2933, .T. ) ;
#403 = DIRECTION ( 'NONE',  ( 0.000000000000000000, -1.064348848528640545E-29, 1.000000000000000000 ) ) ;
#404 = LINE ( 'NONE', #449, #7910 ) ;
#405 = ORIENTED_EDGE ( 'NONE', *, *, #3410, .F. ) ;
#406 = CARTESIAN_POINT ( 'NONE',  ( 4.000000000000114575, 6.928203230275597591, -8.400000000000018119 ) ) ;
#407 = AXIS2_PLACEMENT_3D ( 'NONE', #5310, #7916, #3997 ) ;
#408 = CARTESIAN_POINT ( 'NONE',  ( -6.686525924292650025, 5.377136764700151339, -8.083279549040247147 ) ) ;
#409 = CARTESIAN_POINT ( 'NONE',  ( 2.560009788482798696E-34, -40.00000000000000711, -120.0000000000000000 ) ) ;
#410 = EDGE_CURVE ( 'NONE', #6592, #4707, #7950, .T. ) ;
#411 =( REPRESENTATION_RELATIONSHIP ('NONE','NONE', #1279, #4603 ) REPRESENTATION_RELATIONSHIP_WITH_TRANSFORMATION ( #7844 )SHAPE_REPRESENTATION_RELATIONSHIP( ) );
#412 = AXIS2_PLACEMENT_3D ( 'NONE', #1063, #3836, #3059 ) ;
#413 = CARTESIAN_POINT ( 'NONE',  ( -4.000000000000114575, -6.928203230275542523, -8.400000000000018119 ) ) ;
#414 = CONICAL_SURFACE ( 'NONE', #3326, 8.000000000000007105, 1.047197551196597631 ) ;
#415 = ORIENTED_EDGE ( 'NONE', *, *, #5873, .T. ) ;
#416 = CIRCLE ( 'NONE', #7358, 15.00000000000002487 ) ;
#417 = CARTESIAN_POINT ( 'NONE',  ( 8.000000000000117240, 3.871967595402003859, -7.901061386767532113 ) ) ;
#418 = CONICAL_SURFACE ( 'NONE', #3188, 8.000000000000007105, 1.047197551196597631 ) ;
#419 = EDGE_LOOP ( 'NONE', ( #3396, #2400 ) ) ;
#420 = VECTOR ( 'NONE', #8328, 1000.000000000000000 ) ;
#421 = CARTESIAN_POINT ( 'NONE',  ( 9.999999999999896971, 0.000000000000000000, 0.000000000000000000 ) ) ;
#422 = ORIENTED_EDGE ( 'NONE', *, *, #2951, .T. ) ;
#423 = DIRECTION ( 'NONE',  ( 0.000000000000000000, 0.000000000000000000, -1.000000000000000000 ) ) ;
#424 = EDGE_CURVE ( 'NONE', #2278, #1504, #1016, .T. ) ;
#425 = VECTOR ( 'NONE', #4592, 1000.000000000000000 ) ;
#426 = DIRECTION ( 'NONE',  ( -6.938893903907228378E-17, 0.000000000000000000, 1.000000000000000000 ) ) ;
#427 = VECTOR ( 'NONE', #3150, 1000.000000000000000 ) ;
#428 = CARTESIAN_POINT ( 'NONE',  ( 4.000000000000003553, 6.928203230275597591, 0.000000000000000000 ) ) ;
#429 = DIRECTION ( 'NONE',  ( 0.000000000000000000, 0.000000000000000000, -1.000000000000000000 ) ) ;
#430 = CARTESIAN_POINT ( 'NONE',  ( 5.500000000000000000, 0.000000000000000000, -50.00000000000000000 ) ) ;
#431 = CIRCLE ( 'NONE', #5289, 4.250000000000010658 ) ;
#432 = CIRCLE ( 'NONE', #8482, 4.000000000000060396 ) ;
#433 = CARTESIAN_POINT ( 'NONE',  ( -7.347286611336967255, -4.995646404165273502, -7.903039949738268177 ) ) ;
#434 = CARTESIAN_POINT ( 'NONE',  ( 7.999999999999340972, -4.618802153516732290, -7.685468820183672278 ) ) ;
#435 = ORIENTED_EDGE ( 'NONE', *, *, #2401, .T. ) ;
#436 = PRODUCT_DEFINITION_SHAPE ( 'NONE', 'NONE',  #8635 ) ;
#437 = DIRECTION ( 'NONE',  ( -1.000000000000000000, -2.775557561562916200E-15, 0.000000000000000000 ) ) ;
#438 = ORIENTED_EDGE ( 'NONE', *, *, #4062, .T. ) ;
#439 = ADVANCED_FACE ( 'NONE', ( #590 ), #6765, .F. ) ;
#440 = CARTESIAN_POINT ( 'NONE',  ( 8.000000000000007105, 7.960204194471028619E-16, -6.499999999999334754 ) ) ;
#441 = CARTESIAN_POINT ( 'NONE',  ( 10.00000000000000888, -650.0000000000002274, 79.99999999999995737 ) ) ;
#442 = ORIENTED_EDGE ( 'NONE', *, *, #3742, .F. ) ;
#443 = ORIENTED_EDGE ( 'NONE', *, *, #4512, .F. ) ;
#444 = DIRECTION ( 'NONE',  ( 1.000000000000000000, 8.881784197001244435E-16, 0.000000000000000000 ) ) ;
#445 = EDGE_CURVE ( 'NONE', #1642, #1712, #1258, .T. ) ;
#446 = UNCERTAINTY_MEASURE_WITH_UNIT (LENGTH_MEASURE( 1.000000000000000082E-05 ), #3151, 'distance_accuracy_value', 'NONE');
#447 = DIRECTION ( 'NONE',  ( 6.400024471207029615E-36, -1.000000000000000000, 0.000000000000000000 ) ) ;
#448 = DIRECTION ( 'NONE',  ( -6.400024471207028278E-36, 1.000000000000000000, 0.000000000000000000 ) ) ;
#449 = CARTESIAN_POINT ( 'NONE',  ( 33.00000000000055422, -1.431146867680869324E-14, 3.309500000006883269 ) ) ;
#450 = VERTEX_POINT ( 'NONE', #1353 ) ;
#451 = CARTESIAN_POINT ( 'NONE',  ( -8.000000000000673239, 4.618802153517287401, -7.685468820183672278 ) ) ;
#452 = EDGE_CURVE ( 'NONE', #3139, #799, #6073, .T. ) ;
#453 = DIRECTION ( 'NONE',  ( -1.000000000000000000, 6.572520305780926719E-14, 0.000000000000000000 ) ) ;
#454 = APPLICATION_PROTOCOL_DEFINITION ( 'draft international standard', 'automotive_design', 1998, #4636 ) ;
#455 = EDGE_CURVE ( 'NONE', #2278, #7258, #7612, .T. ) ;
#456 = CARTESIAN_POINT ( 'NONE',  ( -4.681481898396970820, 6.534749472788062619, -8.400000000000073186 ) ) ;
#457 = CIRCLE ( 'NONE', #6440, 80.00000000000001421 ) ;
#458 = CARTESIAN_POINT ( 'NONE',  ( 10.00000000000000888, -0.8578643762688908936, 0.000000000000000000 ) ) ;
#459 = EDGE_LOOP ( 'NONE', ( #7143, #3679, #3302, #4348, #6214, #8113 ) ) ;
#460 = CYLINDRICAL_SURFACE ( 'NONE', #6966, 75.00000000000005684 ) ;
#461 = CIRCLE ( 'NONE', #2535, 4.499999999999993783 ) ;
#462 = VERTEX_POINT ( 'NONE', #2562 ) ;
#463 = CIRCLE ( 'NONE', #312, 5.000000000000069278 ) ;
#464 = CARTESIAN_POINT ( 'NONE',  ( -2.644994884458949702, 7.710515798486381023, -0.08224679563969222729 ) ) ;
#465 = ORIENTED_EDGE ( 'NONE', *, *, #5590, .T. ) ;
#466 = DIRECTION ( 'NONE',  ( 0.000000000000000000, 0.4999999999999986677, -0.8660254037844393737 ) ) ;
#467 = CARTESIAN_POINT ( 'NONE',  ( 1.163414459189985288E-15, -9.500000000000001776, 130.0000000000000000 ) ) ;
#468 = AXIS2_PLACEMENT_3D ( 'NONE', #4578, #1260, #4007 ) ;
#469 = CARTESIAN_POINT ( 'NONE',  ( -8.000000000000229150, 4.440892098500626162E-13, -8.400000000000018119 ) ) ;
#470 = FACE_OUTER_BOUND ( 'NONE', #349, .T. ) ;
#471 = CARTESIAN_POINT ( 'NONE',  ( 2.477984895244330595E-45, 6.980486755139308644E-16, 5.700000000000001954 ) ) ;
#472 = FACE_OUTER_BOUND ( 'NONE', #4653, .T. ) ;
#473 = CIRCLE ( 'NONE', #3101, 10.50000000000001066 ) ;
#474 = ADVANCED_FACE ( 'NONE', ( #7871 ), #5260, .F. ) ;
#475 = LINE ( 'NONE', #5807, #2024 ) ;
#476 = DIRECTION ( 'NONE',  ( 1.000000000000000000, 0.000000000000000000, 0.000000000000000000 ) ) ;
#477 = VERTEX_POINT ( 'NONE', #2037 ) ;
#478 = ORIENTED_EDGE ( 'NONE', *, *, #4857, .F. ) ;
#479 = AXIS2_PLACEMENT_3D ( 'NONE', #3533, #253, #2914 ) ;
#480 = CONICAL_SURFACE ( 'NONE', #3807, 75.00000000000005684, 0.7853981633974441712 ) ;
#481 = AXIS2_PLACEMENT_3D ( 'NONE', #8291, #2277, #4190 ) ;
#482 = DIRECTION ( 'NONE',  ( 1.463706757734299248E-32, -1.000000000000000000, -5.238529448733281520E-32 ) ) ;
#483 = DIRECTION ( 'NONE',  ( 0.000000000000000000, -1.064348848528640545E-29, 1.000000000000000000 ) ) ;
#484 = VERTEX_POINT ( 'NONE', #6614 ) ;
#485 = EDGE_CURVE ( 'NONE', #7120, #4330, #2916, .T. ) ;
#486 = ORIENTED_EDGE ( 'NONE', *, *, #7335, .T. ) ;
#487 = CARTESIAN_POINT ( 'NONE',  ( -8.000000000000007105, 1.110223024625156540E-13, 0.000000000000000000 ) ) ;
#488 = PRODUCT_DEFINITION_FORMATION_WITH_SPECIFIED_SOURCE ( 'ANY', '', #5218, .NOT_KNOWN. ) ;
#489 = CARTESIAN_POINT ( 'NONE',  ( 0.000000000000000000, 0.000000000000000000, 18.00000000000000355 ) ) ;
#490 = DIRECTION ( 'NONE',  ( 0.000000000000000000, 0.000000000000000000, -1.000000000000000000 ) ) ;
#491 = PLANE ( 'NONE',  #5476 ) ;
#492 = CARTESIAN_POINT ( 'NONE',  ( -14.24999999999983125, 15.00000000000014211, 10.00000000000000888 ) ) ;
#493 = EDGE_LOOP ( 'NONE', ( #6950, #6237, #3890, #3563, #7554, #2080 ) ) ;
#494 = EDGE_CURVE ( 'NONE', #3910, #4142, #3557, .T. ) ;
#495 = LINE ( 'NONE', #5274, #5177 ) ;
#496 = CARTESIAN_POINT ( 'NONE',  ( 5.000000000000115463, 2.342598717236854977, -4.057500000000047180 ) ) ;
#497 = DIRECTION ( 'NONE',  ( -1.000000000000000000, -8.881784197001244435E-16, 0.000000000000000000 ) ) ;
#498 = EDGE_CURVE ( 'NONE', #173, #232, #3606, .T. ) ;
#499 = DIRECTION ( 'NONE',  ( -7.703719777548943412E-34, 0.000000000000000000, 1.000000000000000000 ) ) ;
#500 = ORIENTED_EDGE ( 'NONE', *, *, #647, .F. ) ;
#501 = DIRECTION ( 'NONE',  ( -6.409494854920720919E-30, 0.8660254037844380415, -0.5000000000000009992 ) ) ;
#502 = ORIENTED_EDGE ( 'NONE', *, *, #6495, .T. ) ;
#503 = CARTESIAN_POINT ( 'NONE',  ( 3.999999999999559464, 6.928203230274987412, -8.400000000000018119 ) ) ;
#504 = ORIENTED_EDGE ( 'NONE', *, *, #3487, .F. ) ;
#505 = AXIS2_PLACEMENT_3D ( 'NONE', #1191, #6397, #7652 ) ;
#506 = LINE ( 'NONE', #337, #7415 ) ;
#507 = CARTESIAN_POINT ( 'NONE',  ( 0.000000000000000000, 0.000000000000000000, 0.000000000000000000 ) ) ;
#508 = DIRECTION ( 'NONE',  ( -1.000000000000000000, -8.881784197001244435E-16, 0.000000000000000000 ) ) ;
#509 = FACE_OUTER_BOUND ( 'NONE', #3864, .T. ) ;
#510 = FACE_OUTER_BOUND ( 'NONE', #7059, .T. ) ;
#511 = FACE_BOUND ( 'NONE', #2259, .T. ) ;
#512 = EDGE_LOOP ( 'NONE', ( #2319, #8430 ) ) ;
#513 =( LENGTH_UNIT ( ) NAMED_UNIT ( * ) SI_UNIT ( .MILLI., .METRE. ) );
#514 = ORIENTED_EDGE ( 'NONE', *, *, #4418, .T. ) ;
#515 = EDGE_CURVE ( 'NONE', #4124, #4726, #6274, .T. ) ;
#516 = DIRECTION ( 'NONE',  ( 0.000000000000000000, 0.000000000000000000, 1.000000000000000000 ) ) ;
#517 = ITEM_DEFINED_TRANSFORMATION ( 'NONE', 'NONE', #900,  #7563 ) ;
#518 = PLANE ( 'NONE',  #4992 ) ;
#519 = ORIENTED_EDGE ( 'NONE', *, *, #7936, .T. ) ;
#520 = DIRECTION ( 'NONE',  ( 0.000000000000000000, 0.000000000000000000, -1.000000000000000000 ) ) ;
#521 = ORIENTED_EDGE ( 'NONE', *, *, #8538, .T. ) ;
#522 = ADVANCED_FACE ( 'NONE', ( #8225 ), #7611, .F. ) ;
#523 = CARTESIAN_POINT ( 'NONE',  ( -4.339467034331338624, -6.732211846623388674, -8.399999999999982592 ) ) ;
#524 = CARTESIAN_POINT ( 'NONE',  ( 0.000000000000000000, -294.9999999999998295, -2.775557561562891351E-14 ) ) ;
#525 = CARTESIAN_POINT ( 'NONE',  ( -8.000000000000229150, 4.440892098500626162E-13, -8.400000000000018119 ) ) ;
#526 = PRESENTATION_STYLE_ASSIGNMENT (( #7152 ) ) ;
#527 = EDGE_LOOP ( 'NONE', ( #6886, #2691, #1406, #7538 ) ) ;
#528 =( LENGTH_UNIT ( ) NAMED_UNIT ( * ) SI_UNIT ( .MILLI., .METRE. ) );
#529 = EDGE_CURVE ( 'NONE', #7606, #3196, #1630, .T. ) ;
#530 = VERTEX_POINT ( 'NONE', #3474 ) ;
#531 = CIRCLE ( 'NONE', #121, 8.000000000000007105 ) ;
#532 = LINE ( 'NONE', #5149, #5435 ) ;
#533 = CARTESIAN_POINT ( 'NONE',  ( -8.000000000000007105, 4.618802153517009401, -8.400000000000018119 ) ) ;
#534 = ORIENTED_EDGE ( 'NONE', *, *, #219, .F. ) ;
#535 = EDGE_CURVE ( 'NONE', #6830, #5405, #2458, .T. ) ;
#536 = ADVANCED_FACE ( 'NONE', ( #7444 ), #6518, .T. ) ;
#537 = DIRECTION ( 'NONE',  ( 0.8660254037844367092, -0.5000000000000033307, 0.000000000000000000 ) ) ;
#538 = EDGE_LOOP ( 'NONE', ( #1198, #7491, #4676, #8222 ) ) ;
#539 = DIRECTION ( 'NONE',  ( -0.000000000000000000, -1.000000000000000000, -0.000000000000000000 ) ) ;
#540 = PRODUCT_DEFINITION_CONTEXT ( 'detailed design', #5188, 'design' ) ;
#541 = CIRCLE ( 'NONE', #3878, 5.000000000000069278 ) ;
#542 = AXIS2_PLACEMENT_3D ( 'NONE', #3104, #2449, #324 ) ;
#543 = PLANE ( 'NONE',  #4683 ) ;
#544 = DIRECTION ( 'NONE',  ( 1.000000000000000000, 8.881784197001244435E-16, 0.000000000000000000 ) ) ;
#545 = DIRECTION ( 'NONE',  ( 0.000000000000000000, -1.000000000000000000, -7.598173571352217714E-18 ) ) ;
#546 = DIRECTION ( 'NONE',  ( -1.000000000000000000, 1.774937036747276562E-30, 0.000000000000000000 ) ) ;
#547 = ORIENTED_EDGE ( 'NONE', *, *, #2475, .T. ) ;
#548 = CIRCLE ( 'NONE', #5427, 4.499999999999983125 ) ;
#549 = ORIENTED_EDGE ( 'NONE', *, *, #1644, .T. ) ;
#550 = LINE ( 'NONE', #5350, #242 ) ;
#551 = AXIS2_PLACEMENT_3D ( 'NONE', #7520, #6310, #6955 ) ;
#552 = PRODUCT ( 'Servo motor', 'Servo motor', '', ( #3975 ) ) ;
#553 = CARTESIAN_POINT ( 'NONE',  ( 0.6543471694410692985, 8.859816792613512959, -0.4964154566687120074 ) ) ;
#554 = ITEM_DEFINED_TRANSFORMATION ( 'NONE', 'NONE', #4373,  #7563 ) ;
#555 = ORIENTED_EDGE ( 'NONE', *, *, #3272, .T. ) ;
#556 = CARTESIAN_POINT ( 'NONE',  ( 8.000000000000229150, -1.665334536937734811E-13, -8.400000000000018119 ) ) ;
#557 = ORIENTED_EDGE ( 'NONE', *, *, #5105, .F. ) ;
#558 = EDGE_CURVE ( 'NONE', #4476, #8418, #2901, .T. ) ;
#559 = EDGE_CURVE ( 'NONE', #3935, #2131, #2494, .T. ) ;
#560 = ORIENTED_EDGE ( 'NONE', *, *, #1216, .F. ) ;
#561 = AXIS2_PLACEMENT_3D ( 'NONE', #209, #4875, #2869 ) ;
#562 = CARTESIAN_POINT ( 'NONE',  ( 0.000000000000000000, -32.50000000000004974, 0.000000000000000000 ) ) ;
#563 = ORIENTED_EDGE ( 'NONE', *, *, #6140, .T. ) ;
#564 = LINE ( 'NONE', #5822, #7147 ) ;
#565 = LINE ( 'NONE', #5367, #5443 ) ;
#566 = CARTESIAN_POINT ( 'NONE',  ( 4.000000000000003553, -1.759474945355333109, 3.047500000000091802 ) ) ;
#567 = CARTESIAN_POINT ( 'NONE',  ( -8.000000000000007105, -4.618802153517065356, -0.7145311798163467287 ) ) ;
#568 = CARTESIAN_POINT ( 'NONE',  ( 0.000000000000000000, 0.000000000000000000, -8.400000000000018119 ) ) ;
#569 = VERTEX_POINT ( 'NONE', #6106 ) ;
#570 = CARTESIAN_POINT ( 'NONE',  ( 0.000000000000000000, 0.000000000000000000, -8.400000000000018119 ) ) ;
#571 = EDGE_CURVE ( 'NONE', #3965, #8336, #5577, .T. ) ;
#572 = ITEM_DEFINED_TRANSFORMATION ( 'NONE', 'NONE', #2160,  #7563 ) ;
#573 = DIRECTION ( 'NONE',  ( 3.919652622816902408E-30, 3.944304526105059027E-30, -1.000000000000000000 ) ) ;
#574 = ORIENTED_EDGE ( 'NONE', *, *, #8507, .T. ) ;
#575 = CARTESIAN_POINT ( 'NONE',  ( -45.49999999999968026, 87.50000000000036948, -1.942890293094023693E-13 ) ) ;
#576 = EDGE_CURVE ( 'NONE', #3286, #2515, #327, .T. ) ;
#577 = FACE_OUTER_BOUND ( 'NONE', #538, .T. ) ;
#578 = CARTESIAN_POINT ( 'NONE',  ( 0.000000000000000000, 0.000000000000000000, 0.000000000000000000 ) ) ;
#579 = VERTEX_POINT ( 'NONE', #822 ) ;
#580 = AXIS2_PLACEMENT_3D ( 'NONE', #4509, #3851, #2423 ) ;
#581 = CIRCLE ( 'NONE', #5462, 15.00000000000000355 ) ;
#582 = CARTESIAN_POINT ( 'NONE',  ( 0.6543471694410680772, 8.859816792613512959, -7.903584543331305667 ) ) ;
#583 = ORIENTED_EDGE ( 'NONE', *, *, #3619, .F. ) ;
#584 = CARTESIAN_POINT ( 'NONE',  ( -8.000000000000007105, -4.618802153517065356, -0.7145311798163467287 ) ) ;
#585 = AXIS2_PLACEMENT_3D ( 'NONE', #5412, #4182, #1358 ) ;
#586 = DIRECTION ( 'NONE',  ( -1.000000000000000000, 0.000000000000000000, 0.000000000000000000 ) ) ;
#587 = LINE ( 'NONE', #3243, #4960 ) ;
#588 = CARTESIAN_POINT ( 'NONE',  ( 5.000000000000004441, -4.685197434473812095, 0.000000000000000000 ) ) ;
#589 = CIRCLE ( 'NONE', #7410, 5.500000000000023981 ) ;
#590 = FACE_OUTER_BOUND ( 'NONE', #2757, .T. ) ;
#591 = CARTESIAN_POINT ( 'NONE',  ( -82.49999999999945999, 120.0000000000003268, 10.00000000000000888 ) ) ;
#592 = EDGE_CURVE ( 'NONE', #6230, #3933, #4357, .T. ) ;
#593 = CARTESIAN_POINT ( 'NONE',  ( 10.40000000000001990, 6.123233995732941293E-16, -4.999999999999590550 ) ) ;
#594 = ORIENTED_EDGE ( 'NONE', *, *, #4710, .T. ) ;
#595 = DIRECTION ( 'NONE',  ( -3.851859888774471706E-33, 7.598173571352223877E-18, -1.000000000000000000 ) ) ;
#596 = ORIENTED_EDGE ( 'NONE', *, *, #7934, .T. ) ;
#597 = CARTESIAN_POINT ( 'NONE',  ( -4.000000000000891731, 6.928203230275542523, -8.400000000000018119 ) ) ;
#598 = AXIS2_PLACEMENT_3D ( 'NONE', #1093, #1261, #3795 ) ;
#599 = CIRCLE ( 'NONE', #8258, 70.00000000000008527 ) ;
#600 = FACE_OUTER_BOUND ( 'NONE', #8283, .T. ) ;
#601 = CARTESIAN_POINT ( 'NONE',  ( -8.000000000000220268, -1.555946510856261567, -0.06708870216349256677 ) ) ;
#602 = VECTOR ( 'NONE', #6763, 1000.000000000000000 ) ;
#603 = CARTESIAN_POINT ( 'NONE',  ( 0.000000000000000000, -294.9999999999998295, 75.00000000000002842 ) ) ;
#604 = CARTESIAN_POINT ( 'NONE',  ( -7.999999999999896083, 3.871967595402076689, -7.901061386767628925 ) ) ;
#605 = VERTEX_POINT ( 'NONE', #5445 ) ;
#606 = CARTESIAN_POINT ( 'NONE',  ( 4.000000000000225597, -6.928203230275542523, -8.400000000000018119 ) ) ;
#607 = ORIENTED_EDGE ( 'NONE', *, *, #3193, .T. ) ;
#608 = EDGE_LOOP ( 'NONE', ( #1418, #8294, #5860, #146 ) ) ;
#609 = AXIS2_PLACEMENT_3D ( 'NONE', #6883, #912, #953 ) ;
#610 = B_SPLINE_CURVE_WITH_KNOTS ( 'NONE', 3,
 ( #103, #7440, #820, #1470, #152, #5802, #5108, #3694 ),
 .UNSPECIFIED., .F., .F.,
 ( 4, 2, 2, 4 ),
 ( 0.004673709593151774075, 0.005837709341827349366, 0.007001709090502924657, 0.009329708587854076973 ),
 .UNSPECIFIED. ) ;
#611 = CARTESIAN_POINT ( 'NONE',  ( -5.080504117408895404, -2.106769544347820933, 0.000000000000000000 ) ) ;
#612 = ORIENTED_EDGE ( 'NONE', *, *, #2401, .F. ) ;
#613 = CARTESIAN_POINT ( 'NONE',  ( -8.000000000000673239, 4.618802153517287401, -0.7145311798163467287 ) ) ;
#614 = CARTESIAN_POINT ( 'NONE',  ( 275.0000000000000000, 425.0000000000000000, 1.561424668912875158E-13 ) ) ;
#615 = DIRECTION ( 'NONE',  ( 1.000000000000000000, 0.000000000000000000, 0.000000000000000000 ) ) ;
#616 = DIRECTION ( 'NONE',  ( -1.000000000000000000, 0.000000000000000000, 0.000000000000000000 ) ) ;
#617 = ORIENTED_EDGE ( 'NONE', *, *, #410, .F. ) ;
#618 = AXIS2_PLACEMENT_3D ( 'NONE', #6780, #2977, #8123 ) ;
#619 = DIRECTION ( 'NONE',  ( 0.000000000000000000, -0.4999999999999989453, 0.8660254037844392627 ) ) ;
#620 = SHAPE_DEFINITION_REPRESENTATION ( #629, #5209 ) ;
#621 = DIRECTION ( 'NONE',  ( -1.000000000000000000, 0.000000000000000000, 0.000000000000000000 ) ) ;
#622 = CARTESIAN_POINT ( 'NONE',  ( 5.000000000000004441, 0.000000000000000000, 0.000000000000000000 ) ) ;
#623 = EDGE_CURVE ( 'NONE', #2349, #7854, #2821, .T. ) ;
#624 = ORIENTED_EDGE ( 'NONE', *, *, #8030, .T. ) ;
#625 = CARTESIAN_POINT ( 'NONE',  ( -8.000000000000007105, 0.000000000000000000, 0.000000000000000000 ) ) ;
#626 =( NAMED_UNIT ( * ) SI_UNIT ( $, .STERADIAN. ) SOLID_ANGLE_UNIT ( ) );
#627 = ORIENTED_EDGE ( 'NONE', *, *, #1962, .T. ) ;
#628 = CARTESIAN_POINT ( 'NONE',  ( 0.000000000000000000, 0.000000000000000000, 0.000000000000000000 ) ) ;
#629 = PRODUCT_DEFINITION_SHAPE ( 'NONE', 'NONE',  #2753 ) ;
#630 = ORIENTED_EDGE ( 'NONE', *, *, #1968, .T. ) ;
#631 = CARTESIAN_POINT ( 'NONE',  ( -31.74999999999994316, 4.898587196589875298E-16, -4.000000000000030198 ) ) ;
#632 = EDGE_CURVE ( 'NONE', #6090, #6584, #2176, .T. ) ;
#633 = PLANE ( 'NONE',  #383 ) ;
#634 = CARTESIAN_POINT ( 'NONE',  ( 4.250000000000008882, -32.50000000000004974, 18.00000000000000355 ) ) ;
#635 = CARTESIAN_POINT ( 'NONE',  ( -3.318518101603071369, -7.321656987762848345, 3.872634634846659572E-15 ) ) ;
#636 = CARTESIAN_POINT ( 'NONE',  ( -44.99999999999992895, 500.0000000000000000, -45.00000000000000711 ) ) ;
#637 = DIRECTION ( 'NONE',  ( 0.000000000000000000, 0.000000000000000000, 1.000000000000000000 ) ) ;
#638 = ORIENTED_EDGE ( 'NONE', *, *, #7578, .F. ) ;
#639 = PLANE ( 'NONE',  #6979 ) ;
#640 = EDGE_LOOP ( 'NONE', ( #7745, #1073, #1566, #6105 ) ) ;
#641 = DIRECTION ( 'NONE',  ( 0.000000000000000000, 0.000000000000000000, 1.000000000000000000 ) ) ;
#642 = AXIS2_PLACEMENT_3D ( 'NONE', #2902, #2253, #6469 ) ;
#643 = EDGE_CURVE ( 'NONE', #5503, #8027, #3386, .T. ) ;
#644 = CARTESIAN_POINT ( 'NONE',  ( -275.0000000000000000, 425.0000000000000000, 75.00000000000015632 ) ) ;
#645 = CARTESIAN_POINT ( 'NONE',  ( -4.000000000000003553, 6.928203230275431501, 0.000000000000000000 ) ) ;
#646 = CONTEXT_DEPENDENT_SHAPE_REPRESENTATION ( #2391, #4396 ) ;
#647 = EDGE_CURVE ( 'NONE', #2499, #2290, #7527, .T. ) ;
#648 = FACE_OUTER_BOUND ( 'NONE', #286, .T. ) ;
#649 = CARTESIAN_POINT ( 'NONE',  ( -6.686525924292996415, 5.377136764700138016, -8.083279549040094381 ) ) ;
#650 = VERTEX_POINT ( 'NONE', #7651 ) ;
#651 = CARTESIAN_POINT ( 'NONE',  ( -36.74999999999997158, 3.469446951953614189E-15, 18.00000000000000355 ) ) ;
#652 = ORIENTED_EDGE ( 'NONE', *, *, #8538, .F. ) ;
#653 = EDGE_CURVE ( 'NONE', #369, #7541, #599, .T. ) ;
#654 = DIRECTION ( 'NONE',  ( 0.000000000000000000, -1.064348848528640545E-29, 1.000000000000000000 ) ) ;
#655 = ORIENTED_EDGE ( 'NONE', *, *, #7198, .T. ) ;
#656 = FACE_OUTER_BOUND ( 'NONE', #3276, .T. ) ;
#657 = DIRECTION ( 'NONE',  ( 3.919652622816902408E-30, 3.944304526105059027E-30, -1.000000000000000000 ) ) ;
#658 = CARTESIAN_POINT ( 'NONE',  ( -82.49999999999945999, 120.0000000000003268, 10.00000000000000888 ) ) ;
#659 = AXIS2_PLACEMENT_3D ( 'NONE', #2516, #3903, #4518 ) ;
#660 = DIRECTION ( 'NONE',  ( 0.000000000000000000, 1.064348848528640545E-29, -1.000000000000000000 ) ) ;
#661 =( NAMED_UNIT ( * ) SI_UNIT ( $, .STERADIAN. ) SOLID_ANGLE_UNIT ( ) );
#662 = VERTEX_POINT ( 'NONE', #5028 ) ;
#663 = DIRECTION ( 'NONE',  ( 0.000000000000000000, 0.000000000000000000, 1.000000000000000000 ) ) ;
#664 = APPLICATION_PROTOCOL_DEFINITION ( 'draft international standard', 'automotive_design', 1998, #7088 ) ;
#665 = ADVANCED_FACE ( 'NONE', ( #7690 ), #1718, .F. ) ;
#666 = ORIENTED_EDGE ( 'NONE', *, *, #745, .T. ) ;
#667 = CARTESIAN_POINT ( 'NONE',  ( -4.250000000000008882, -32.50000000000004974, 18.00000000000000355 ) ) ;
#668 = DIRECTION ( 'NONE',  ( 1.463706757734299248E-32, -1.000000000000000000, -5.238529448733281520E-32 ) ) ;
#669 =( NAMED_UNIT ( * ) PLANE_ANGLE_UNIT ( ) SI_UNIT ( $, .RADIAN. ) );
#670 = ORIENTED_EDGE ( 'NONE', *, *, #5204, .T. ) ;
#671 = PRESENTATION_STYLE_ASSIGNMENT (( #3153 ) ) ;
#672 = EDGE_CURVE ( 'NONE', #704, #605, #506, .T. ) ;
#673 = ADVANCED_FACE ( 'NONE', ( #2459 ), #4086, .T. ) ;
#674 = FACE_OUTER_BOUND ( 'NONE', #7400, .T. ) ;
#675 = ORIENTED_EDGE ( 'NONE', *, *, #6201, .T. ) ;
#676 = CARTESIAN_POINT ( 'NONE',  ( 7.999999999999674039, -4.618802153517231446, -7.685468820183672278 ) ) ;
#677 = B_SPLINE_CURVE_WITH_KNOTS ( 'NONE', 3,
 ( #1730, #6481, #3131, #8524, #3748, #2565 ),
 .UNSPECIFIED., .F., .F.,
 ( 4, 2, 4 ),
 ( 2.380731628247534354E-07, 0.002336973833157795794, 0.004673709593152765469 ),
 .UNSPECIFIED. ) ;
#678 = LINE ( 'NONE', #5249, #6920 ) ;
#679 = CARTESIAN_POINT ( 'NONE',  ( -6.080023247646675662E-35, 9.499999999999994671, 130.0000000000000000 ) ) ;
#680 = DIRECTION ( 'NONE',  ( 0.000000000000000000, 0.000000000000000000, -1.000000000000000000 ) ) ;
#681 = CARTESIAN_POINT ( 'NONE',  ( -5.499999999999999112, 60.00000000000000000, -50.00000000000000000 ) ) ;
#682 = DIRECTION ( 'NONE',  ( -1.000000000000000000, -0.000000000000000000, -0.000000000000000000 ) ) ;
#683 = VERTEX_POINT ( 'NONE', #6965 ) ;
#684 = ADVANCED_FACE ( 'NONE', ( #8308 ), #1670, .T. ) ;
#685 = SURFACE_STYLE_USAGE ( .BOTH. , #6608 ) ;
#686 = LINE ( 'NONE', #6066, #6271 ) ;
#687 = DIRECTION ( 'NONE',  ( 1.000000000000000000, 8.881784197001244435E-16, 0.000000000000000000 ) ) ;
#688 = CIRCLE ( 'NONE', #5560, 8.000000000000007105 ) ;
#689 = CIRCLE ( 'NONE', #1791, 19.49999999999996803 ) ;
#690 = CARTESIAN_POINT ( 'NONE',  ( -3.999999999999892530, 6.928203230275431501, 0.000000000000000000 ) ) ;
#691 = CIRCLE ( 'NONE', #4027, 10.00000000000000178 ) ;
#692 = DIRECTION ( 'NONE',  ( 0.000000000000000000, -0.000000000000000000, 1.000000000000000000 ) ) ;
#693 = AXIS2_PLACEMENT_3D ( 'NONE', #6436, #3122, #5806 ) ;
#694 = DIRECTION ( 'NONE',  ( -3.919652622816902408E-30, -3.944304526105059027E-30, 1.000000000000000000 ) ) ;
#695 = ORIENTED_EDGE ( 'NONE', *, *, #4152, .T. ) ;
#696 = ADVANCED_FACE ( 'NONE', ( #5758, #8388, #999 ), #4341, .F. ) ;
#697 = PRESENTATION_STYLE_ASSIGNMENT (( #8144 ) ) ;
#698 = VERTEX_POINT ( 'NONE', #7008 ) ;
#699 = CARTESIAN_POINT ( 'NONE',  ( 0.000000000000000000, -2.342598717236902939, 4.057500000000047180 ) ) ;
#700 = DIRECTION ( 'NONE',  ( -1.000000000000000000, -0.000000000000000000, -0.000000000000000000 ) ) ;
#701 = COLOUR_RGB ( '',0.7921568627450980005, 0.8196078431372548767, 0.9333333333333333481 ) ;
#702 = CARTESIAN_POINT ( 'NONE',  ( -8.000000000000220268, -1.555946510856260012, -8.332911297836524511 ) ) ;
#703 = DIRECTION ( 'NONE',  ( 0.000000000000000000, 0.000000000000000000, 1.000000000000000000 ) ) ;
#704 = VERTEX_POINT ( 'NONE', #8349 ) ;
#705 = B_SPLINE_CURVE_WITH_KNOTS ( 'NONE', 3,
 ( #1623, #2857, #7561, #4159, #4251, #6265, #2939, #2287 ),
 .UNSPECIFIED., .F., .F.,
 ( 4, 2, 2, 4 ),
 ( 0.004673709593151987446, 0.005837709341827518501, 0.007001709090503049557, 0.009329708587854111668 ),
 .UNSPECIFIED. ) ;
#706 = ORIENTED_EDGE ( 'NONE', *, *, #1007, .T. ) ;
#707 = MECHANICAL_DESIGN_GEOMETRIC_PRESENTATION_REPRESENTATION (  '', ( #5446 ), #1666 ) ;
#708 = EDGE_CURVE ( 'NONE', #8288, #1229, #2420, .T. ) ;
#709 = SHAPE_DEFINITION_REPRESENTATION ( #3889, #7270 ) ;
#710 = EDGE_CURVE ( 'NONE', #6028, #749, #1114, .T. ) ;
#711 = DIRECTION ( 'NONE',  ( -1.000000000000000000, 0.000000000000000000, 6.938893903907228378E-17 ) ) ;
#712 = ORIENTED_EDGE ( 'NONE', *, *, #1927, .T. ) ;
#713 = CARTESIAN_POINT ( 'NONE',  ( 8.000000000000232703, 3.115336682266936830, -8.080606868608402493 ) ) ;
#714 = CARTESIAN_POINT ( 'NONE',  ( 350.0000000000000568, -1.194553624853794682E-13, -4.163336342344337027E-14 ) ) ;
#715 = ORIENTED_EDGE ( 'NONE', *, *, #8367, .T. ) ;
#716 = ADVANCED_FACE ( 'NONE', ( #5109, #6318 ), #7768, .F. ) ;
#717 = DIRECTION ( 'NONE',  ( 2.775557561562879124E-15, 1.000000000000000000, 3.944304526105070237E-30 ) ) ;
#718 = ORIENTED_EDGE ( 'NONE', *, *, #558, .T. ) ;
#719 = DIRECTION ( 'NONE',  ( 6.938893903907228378E-17, 0.000000000000000000, -1.000000000000000000 ) ) ;
#720 = CARTESIAN_POINT ( 'NONE',  ( 0.000000000000000000, 60.00000000000000000, -50.00000000000000000 ) ) ;
#721 = DIRECTION ( 'NONE',  ( -3.851859888774471706E-33, -1.232595164407830946E-32, -1.000000000000000000 ) ) ;
#722 = CARTESIAN_POINT ( 'NONE',  ( 8.000000000000008882, 1.572549600175326745, -8.331055444744915661 ) ) ;
#723 = CARTESIAN_POINT ( 'NONE',  ( -8.000000000000671463, 3.871967595402323603, -0.4989386132328571533 ) ) ;
#724 = VECTOR ( 'NONE', #6940, 1000.000000000000000 ) ;
#725 = CARTESIAN_POINT ( 'NONE',  ( -4.339467034331342177, -6.732211846623386897, -3.613251970573713029E-14 ) ) ;
#726 = ORIENTED_EDGE ( 'NONE', *, *, #4374, .T. ) ;
#727 = FACE_BOUND ( 'NONE', #4525, .T. ) ;
#728 = DIRECTION ( 'NONE',  ( 0.000000000000000000, -1.042965139114318396E-29, 1.000000000000000000 ) ) ;
#729 = FACE_OUTER_BOUND ( 'NONE', #7779, .T. ) ;
#730 = CONICAL_SURFACE ( 'NONE', #5761, 38.74999999999999289, 0.7853981633974447263 ) ;
#731 = LINE ( 'NONE', #3391, #359 ) ;
#732 = EDGE_CURVE ( 'NONE', #3003, #1200, #8389, .T. ) ;
#733 = VECTOR ( 'NONE', #5528, 1000.000000000000114 ) ;
#734 = CARTESIAN_POINT ( 'NONE',  ( -3.660532965669041516, 7.124194613927598674, -8.399999999999977263 ) ) ;
#735 = CARTESIAN_POINT ( 'NONE',  ( -8.000000000000229150, 3.871967595402046491, -7.901061386767464612 ) ) ;
#736 = ORIENTED_EDGE ( 'NONE', *, *, #8068, .T. ) ;
#737 = SURFACE_SIDE_STYLE ('',( #7352 ) ) ;
#738 = ORIENTED_EDGE ( 'NONE', *, *, #219, .T. ) ;
#739 = AXIS2_PLACEMENT_3D ( 'NONE', #6687, #717, #91 ) ;
#740 = DIRECTION ( 'NONE',  ( -1.000000000000000000, 3.549874073494553124E-30, 0.000000000000000000 ) ) ;
#741 = ORIENTED_EDGE ( 'NONE', *, *, #2143, .F. ) ;
#742 = DIRECTION ( 'NONE',  ( 0.000000000000000000, 0.000000000000000000, -1.000000000000000000 ) ) ;
#743 = CARTESIAN_POINT ( 'NONE',  ( -8.000000000000222045, -3.867591403079426282, -7.902324684675259725 ) ) ;
#744 = CARTESIAN_POINT ( 'NONE',  ( 8.000000000000014211, -5.551115123125777653E-14, -4.399999999999364420 ) ) ;
#745 = EDGE_CURVE ( 'NONE', #3947, #6439, #5046, .T. ) ;
#746 = CIRCLE ( 'NONE', #5638, 19.49999999999996803 ) ;
#747 = FACE_OUTER_BOUND ( 'NONE', #3148, .T. ) ;
#748 = VERTEX_POINT ( 'NONE', #4072 ) ;
#749 = VERTEX_POINT ( 'NONE', #8210 ) ;
#750 = CIRCLE ( 'NONE', #2555, 5.500000000000000000 ) ;
#751 = DIRECTION ( 'NONE',  ( 3.919652622816902408E-30, 3.944304526105059027E-30, -1.000000000000000000 ) ) ;
#752 = AXIS2_PLACEMENT_3D ( 'NONE', #3594, #8249, #139 ) ;
#753 = ADVANCED_FACE ( 'NONE', ( #6740 ), #2810, .F. ) ;
#754 = DIRECTION ( 'NONE',  ( 1.000000000000000000, 8.881784197001244435E-16, 0.000000000000000000 ) ) ;
#755 = EDGE_LOOP ( 'NONE', ( #1822, #2108, #4913 ) ) ;
#756 = CARTESIAN_POINT ( 'NONE',  ( 0.000000000000000000, 0.000000000000000000, 0.000000000000000000 ) ) ;
#757 = VERTEX_POINT ( 'NONE', #938 ) ;
#758 = VERTEX_POINT ( 'NONE', #8599 ) ;
#759 = ADVANCED_FACE ( 'NONE', ( #6786 ), #4895, .F. ) ;
#760 = DIRECTION ( 'NONE',  ( -0.000000000000000000, -0.000000000000000000, 1.000000000000000000 ) ) ;
#761 = ORIENTED_EDGE ( 'NONE', *, *, #8539, .T. ) ;
#762 = CYLINDRICAL_SURFACE ( 'NONE', #8377, 10.00000000000000178 ) ;
#763 = AXIS2_PLACEMENT_3D ( 'NONE', #5818, #6378, #8446 ) ;
#764 = CARTESIAN_POINT ( 'NONE',  ( 0.000000000000000000, 0.000000000000000000, -8.401000000000047763 ) ) ;
#765 = FACE_BOUND ( 'NONE', #1653, .T. ) ;
#766 = EDGE_LOOP ( 'NONE', ( #2291, #6698, #7968, #2471 ) ) ;
#767 = FACE_OUTER_BOUND ( 'NONE', #135, .T. ) ;
#768 = PRODUCT_DEFINITION_SHAPE ( 'NONE', 'NONE',  #8630 ) ;
#769 = EDGE_CURVE ( 'NONE', #6892, #1241, #3931, .T. ) ;
#770 = DIRECTION ( 'NONE',  ( 0.000000000000000000, 0.000000000000000000, -1.000000000000000000 ) ) ;
#771 = CARTESIAN_POINT ( 'NONE',  ( -1.313474075707264488, -8.479269695850916833, -8.083279549040147671 ) ) ;
#772 = ORIENTED_EDGE ( 'NONE', *, *, #8153, .F. ) ;
#773 = FACE_OUTER_BOUND ( 'NONE', #7131, .T. ) ;
#774 =( LENGTH_UNIT ( ) NAMED_UNIT ( * ) SI_UNIT ( .MILLI., .METRE. ) );
#775 = DIRECTION ( 'NONE',  ( 6.400024471206997542E-36, -1.000000000000000000, -7.598173571352217714E-18 ) ) ;
#776 = DIRECTION ( 'NONE',  ( -3.919652622816902408E-30, -3.944304526105059027E-30, 1.000000000000000000 ) ) ;
#777 = DIRECTION ( 'NONE',  ( -1.000000000000000000, 3.498359009886547695E-15, 3.722437396511637546E-30 ) ) ;
#778 = PRODUCT_DEFINITION_SHAPE ( 'NONE', 'NONE',  #8616 ) ;
#779 = FACE_OUTER_BOUND ( 'NONE', #7734, .T. ) ;
#780 = VECTOR ( 'NONE', #1375, 1000.000000000000000 ) ;
#781 = DIRECTION ( 'NONE',  ( -1.000000000000000000, -8.881784197001244435E-16, 0.000000000000000000 ) ) ;
#782 = CARTESIAN_POINT ( 'NONE',  ( -50.00000000000004263, 425.0000000000000000, 25.00000000000001066 ) ) ;
#783 = ORIENTED_EDGE ( 'NONE', *, *, #3254, .T. ) ;
#784 = CARTESIAN_POINT ( 'NONE',  ( -8.000000000000007105, 4.618802153517009401, -8.400000000000018119 ) ) ;
#785 = EDGE_LOOP ( 'NONE', ( #1709, #6316, #7907 ) ) ;
#786 = EDGE_CURVE ( 'NONE', #1663, #7888, #746, .T. ) ;
#787 = CARTESIAN_POINT ( 'NONE',  ( 5.000000000000004441, -3.513898075855406145, 2.028750000000023590 ) ) ;
#788 = FACE_OUTER_BOUND ( 'NONE', #1413, .T. ) ;
#789 = FACE_OUTER_BOUND ( 'NONE', #5636, .T. ) ;
#790 = ORIENTED_EDGE ( 'NONE', *, *, #7457, .F. ) ;
#791 = DIRECTION ( 'NONE',  ( -1.000000000000000000, 0.000000000000000000, -6.938893903907228378E-17 ) ) ;
#792 = ORIENTED_EDGE ( 'NONE', *, *, #1046, .T. ) ;
#793 = CIRCLE ( 'NONE', #2448, 80.00000000000001421 ) ;
#794 = ORIENTED_EDGE ( 'NONE', *, *, #2912, .F. ) ;
#795 = EDGE_CURVE ( 'NONE', #2499, #6000, #4916, .T. ) ;
#796 = EDGE_CURVE ( 'NONE', #1068, #7820, #6319, .T. ) ;
#797 = CIRCLE ( 'NONE', #4688, 5.500000000000024869 ) ;
#798 = DIRECTION ( 'NONE',  ( 0.000000000000000000, 0.000000000000000000, 1.000000000000000000 ) ) ;
#799 = VERTEX_POINT ( 'NONE', #8449 ) ;
#800 = DIRECTION ( 'NONE',  ( 1.000000000000000000, 0.000000000000000000, 0.000000000000000000 ) ) ;
#801 = CIRCLE ( 'NONE', #5690, 50.00000000000008527 ) ;
#802 = DIRECTION ( 'NONE',  ( -9.860761315262646473E-32, 0.4999999999999988898, -0.8660254037844392627 ) ) ;
#803 = DIRECTION ( 'NONE',  ( 1.000000000000000000, 8.736544766236844851E-16, -1.058471975245250406E-16 ) ) ;
#804 = ORIENTED_EDGE ( 'NONE', *, *, #5681, .F. ) ;
#805 = EDGE_CURVE ( 'NONE', #7820, #1068, #6328, .T. ) ;
#806 = CARTESIAN_POINT ( 'NONE',  ( -8.000000000000003553, -0.7805016046290118581, 5.039846036163083862E-15 ) ) ;
#807 = ORIENTED_EDGE ( 'NONE', *, *, #3230, .F. ) ;
#808 = CARTESIAN_POINT ( 'NONE',  ( 4.681481898396925523, -6.534749472788245583, -8.399999999999996803 ) ) ;
#809 = DIRECTION ( 'NONE',  ( -0.9237280213470678847, -0.3830490080632384942, 0.000000000000000000 ) ) ;
#810 = CARTESIAN_POINT ( 'NONE',  ( 7.999999999999563016, -4.618802153517398423, -0.7145311798163467287 ) ) ;
#811 = ORIENTED_EDGE ( 'NONE', *, *, #1222, .F. ) ;
#812 = AXIS2_PLACEMENT_3D ( 'NONE', #2265, #397, #3583 ) ;
#813 = CARTESIAN_POINT ( 'NONE',  ( 0.000000000000000000, 0.000000000000000000, 45.00000000000000000 ) ) ;
#814 = CARTESIAN_POINT ( 'NONE',  ( -2.300000000000024247, 10.00000000000000888, 0.000000000000000000 ) ) ;
#815 = B_SPLINE_CURVE_WITH_KNOTS ( 'NONE', 3,
 ( #1481, #3403, #3353, #6766, #6964, #7357 ),
 .UNSPECIFIED., .F., .F.,
 ( 4, 2, 4 ),
 ( 0.01291313371729436651, 0.01525081363757299809, 0.01758849355785162966 ),
 .UNSPECIFIED. ) ;
#816 = DIRECTION ( 'NONE',  ( 1.000000000000000000, -0.000000000000000000, -6.938893903907228378E-17 ) ) ;
#817 = EDGE_LOOP ( 'NONE', ( #4283, #4249, #761, #638, #772, #5815 ) ) ;
#818 = FILL_AREA_STYLE_COLOUR ( '', #3766 ) ;
#819 =( NAMED_UNIT ( * ) PLANE_ANGLE_UNIT ( ) SI_UNIT ( $, .RADIAN. ) );
#820 = CARTESIAN_POINT ( 'NONE',  ( -4.680456609903809628, -6.535341423376096692, -0.01688885742794853789 ) ) ;
#821 = AXIS2_PLACEMENT_3D ( 'NONE', #4827, #204, #4216 ) ;
#822 = CARTESIAN_POINT ( 'NONE',  ( 275.0000000000000000, 425.0000000000000000, -74.99999999999984368 ) ) ;
#823 = PLANE ( 'NONE',  #3004 ) ;
#824 = ADVANCED_FACE ( 'NONE', ( #3179 ), #7838, .T. ) ;
#825 = DIRECTION ( 'NONE',  ( -0.9237280213470678847, -0.3830490080632384942, 0.000000000000000000 ) ) ;
#826 = CIRCLE ( 'NONE', #1930, 10.49999999999999645 ) ;
#827 = CARTESIAN_POINT ( 'NONE',  ( -19.99999999999982947, 15.00000000000012434, 10.00000000000000888 ) ) ;
#828 = VERTEX_POINT ( 'NONE', #1919 ) ;
#829 = AXIS2_PLACEMENT_3D ( 'NONE', #8457, #1837, #1102 ) ;
#830 = AXIS2_PLACEMENT_3D ( 'NONE', #5763, #4510, #5888 ) ;
#831 = CARTESIAN_POINT ( 'NONE',  ( -7.999999999999890754, -3.098204225878261386, -0.3157906771918332911 ) ) ;
#832 = ORIENTED_EDGE ( 'NONE', *, *, #6918, .T. ) ;
#833 = CARTESIAN_POINT ( 'NONE',  ( 5.500000000000000000, 0.000000000000000000, -45.00000000000000711 ) ) ;
#834 = DIRECTION ( 'NONE',  ( 0.000000000000000000, -1.064348848528640685E-29, 1.000000000000000000 ) ) ;
#835 = FACE_OUTER_BOUND ( 'NONE', #4264, .T. ) ;
#836 = ORIENTED_EDGE ( 'NONE', *, *, #4162, .F. ) ;
#837 = DIRECTION ( 'NONE',  ( 0.000000000000000000, 0.000000000000000000, 1.000000000000000000 ) ) ;
#838 = VERTEX_POINT ( 'NONE', #4441 ) ;
#839 = ORIENTED_EDGE ( 'NONE', *, *, #2260, .T. ) ;
#840 = CONICAL_SURFACE ( 'NONE', #412, 40.00000000000007816, 0.7853981633974445042 ) ;
#841 = ADVANCED_BREP_SHAPE_REPRESENTATION ( '', ( #2776, #7563 ), #4924 ) ;
#842 = CARTESIAN_POINT ( 'NONE',  ( 0.6527133886632224824, -8.860760056385986516, -0.4969600502619001547 ) ) ;
#843 = DIRECTION ( 'NONE',  ( 4.622231866529366732E-33, -1.224646799147352961E-16, 1.000000000000000000 ) ) ;
#844 = VECTOR ( 'NONE', #6637, 1000.000000000000000 ) ;
#845=STYLED_ITEM('',(#8670),#2776);
#846 = EDGE_CURVE ( 'NONE', #4479, #218, #4939, .T. ) ;
#847 = ORIENTED_EDGE ( 'NONE', *, *, #1734, .T. ) ;
#848 = CARTESIAN_POINT ( 'NONE',  ( 0.000000000000000000, 0.000000000000000000, 50.00000000000000000 ) ) ;
#849 = DIRECTION ( 'NONE',  ( -1.000000000000000222, 1.304512053934558935E-15, 8.476012494971759825E-19 ) ) ;
#850 = ORIENTED_EDGE ( 'NONE', *, *, #6226, .F. ) ;
#851 = ORIENTED_EDGE ( 'NONE', *, *, #7934, .F. ) ;
#852 = DIRECTION ( 'NONE',  ( 1.000000000000000000, 0.000000000000000000, 0.000000000000000000 ) ) ;
#853 =( GEOMETRIC_REPRESENTATION_CONTEXT ( 3 ) GLOBAL_UNCERTAINTY_ASSIGNED_CONTEXT ( ( #3952 ) ) GLOBAL_UNIT_ASSIGNED_CONTEXT ( ( #3224, #1825, #661 ) ) REPRESENTATION_CONTEXT ( 'NONE', 'WORKASPACE' ) );
#854 = EDGE_CURVE ( 'NONE', #1579, #3453, #8518, .T. ) ;
#855 = FACE_OUTER_BOUND ( 'NONE', #3407, .T. ) ;
#856 = EDGE_CURVE ( 'NONE', #7966, #872, #2830, .T. ) ;
#857 = ORIENTED_EDGE ( 'NONE', *, *, #6152, .F. ) ;
#858 = DIRECTION ( 'NONE',  ( 0.000000000000000000, 0.000000000000000000, 1.000000000000000000 ) ) ;
#859 = DIRECTION ( 'NONE',  ( 0.000000000000000000, 0.000000000000000000, -1.000000000000000000 ) ) ;
#860 =( NAMED_UNIT ( * ) PLANE_ANGLE_UNIT ( ) SI_UNIT ( $, .RADIAN. ) );
#861 = EDGE_LOOP ( 'NONE', ( #7328, #4385, #6462, #1916 ) ) ;
#862 =( REPRESENTATION_RELATIONSHIP ('NONE','NONE', #1279, #2536 ) REPRESENTATION_RELATIONSHIP_WITH_TRANSFORMATION ( #4677 )SHAPE_REPRESENTATION_RELATIONSHIP( ) );
#863 = VERTEX_POINT ( 'NONE', #6533 ) ;
#864 = DIRECTION ( 'NONE',  ( 1.000000000000000000, 0.000000000000000000, -6.938893903907228378E-17 ) ) ;
#865 = CARTESIAN_POINT ( 'NONE',  ( 4.000000000000058620, 3.518949890710762585, 2.220446049250313081E-13 ) ) ;
#866 = EDGE_CURVE ( 'NONE', #7532, #232, #8297, .T. ) ;
#867 = CARTESIAN_POINT ( 'NONE',  ( 0.000000000000000000, 4.685197434473812983, 0.000000000000000000 ) ) ;
#868 = CARTESIAN_POINT ( 'NONE',  ( -5.690023276062290414, -5.952467836904619780, -8.269346954796052529 ) ) ;
#869 = DIRECTION ( 'NONE',  ( 3.851859888774471706E-33, -7.598173571352223877E-18, 1.000000000000000000 ) ) ;
#870 = ORIENTED_EDGE ( 'NONE', *, *, #7065, .F. ) ;
#871 = CARTESIAN_POINT ( 'NONE',  ( -8.000000000000666134, -3.098204225877952744, -0.3157906771921843991 ) ) ;
#872 = VERTEX_POINT ( 'NONE', #5909 ) ;
#873 = CIRCLE ( 'NONE', #3915, 5.500000000000024869 ) ;
#874 = DIRECTION ( 'NONE',  ( -1.000000000000000000, -8.881784197001244435E-16, 0.000000000000000000 ) ) ;
#875 = EDGE_CURVE ( 'NONE', #8340, #3886, #3801, .T. ) ;
#876 = VECTOR ( 'NONE', #539, 1000.000000000000000 ) ;
#877 = DIRECTION ( 'NONE',  ( -1.000000000000000000, -0.000000000000000000, -0.000000000000000000 ) ) ;
#878 = DIRECTION ( 'NONE',  ( 0.000000000000000000, -1.064348848528640545E-29, 1.000000000000000000 ) ) ;
#879 = ORIENTED_EDGE ( 'NONE', *, *, #2756, .T. ) ;
#880 = VECTOR ( 'NONE', #1967, 1000.000000000000000 ) ;
#881 = ORIENTED_EDGE ( 'NONE', *, *, #7417, .F. ) ;
#882 = ADVANCED_FACE ( 'NONE', ( #3309 ), #7278, .T. ) ;
#883 = VECTOR ( 'NONE', #4658, 1000.000000000000000 ) ;
#884 = CYLINDRICAL_SURFACE ( 'NONE', #4494, 24.50000000000000000 ) ;
#885 = CONICAL_SURFACE ( 'NONE', #2968, 3.309499999999999886, 0.7853981633975651855 ) ;
#886 = DIRECTION ( 'NONE',  ( 3.919652622816902408E-30, 3.944304526105059027E-30, -1.000000000000000000 ) ) ;
#887 = ORIENTED_EDGE ( 'NONE', *, *, #7094, .T. ) ;
#888 = CIRCLE ( 'NONE', #2697, 8.000000000000007105 ) ;
#889 = PLANE ( 'NONE',  #3626 ) ;
#890 = B_SPLINE_CURVE_WITH_KNOTS ( 'NONE', 3,
 ( #4953, #8139, #7488, #2212, #8228, #5582 ),
 .UNSPECIFIED., .F., .F.,
 ( 4, 2, 4 ),
 ( 2.380731629387024750E-07, 0.002336973833157600638, 0.004673709593152262400 ),
 .UNSPECIFIED. ) ;
#891 = AXIS2_PLACEMENT_3D ( 'NONE', #3001, #5687, #2958 ) ;
#892 = CARTESIAN_POINT ( 'NONE',  ( -5.080504117408895404, -2.106769544347820933, -8.400999999999992696 ) ) ;
#893 = DIRECTION ( 'NONE',  ( 0.000000000000000000, 0.000000000000000000, -1.000000000000000000 ) ) ;
#894 = ORIENTED_EDGE ( 'NONE', *, *, #7114, .T. ) ;
#895 = CARTESIAN_POINT ( 'NONE',  ( 0.000000000000000000, 0.000000000000000000, -8.400999999999992696 ) ) ;
#896 = VERTEX_POINT ( 'NONE', #744 ) ;
#897 = AXIS2_PLACEMENT_3D ( 'NONE', #2889, #852, #2808 ) ;
#898 = FACE_OUTER_BOUND ( 'NONE', #6189, .T. ) ;
#899 = EDGE_CURVE ( 'NONE', #7534, #6851, #5991, .T. ) ;
#900 = AXIS2_PLACEMENT_3D ( 'NONE', #6218, #2885, #5554 ) ;
#901 = CARTESIAN_POINT ( 'NONE',  ( -6.686525924292996415, 5.377136764700138016, -0.3167204509599222950 ) ) ;
#902 = VERTEX_POINT ( 'NONE', #2666 ) ;
#903 = DIRECTION ( 'NONE',  ( 0.000000000000000000, 0.000000000000000000, -1.000000000000000000 ) ) ;
#904 = CARTESIAN_POINT ( 'NONE',  ( 0.000000000000000000, 0.000000000000000000, -8.400000000000018119 ) ) ;
#905 = ORIENTED_EDGE ( 'NONE', *, *, #2015, .F. ) ;
#906 = ORIENTED_EDGE ( 'NONE', *, *, #2537, .F. ) ;
#907 = ADVANCED_FACE ( 'NONE', ( #3404 ), #5334, .T. ) ;
#908 = CARTESIAN_POINT ( 'NONE',  ( -6.689127551062048482, -5.375634714784658819, -8.082649155111331751 ) ) ;
#909 = CARTESIAN_POINT ( 'NONE',  ( 4.000000000000003553, 1.759474945355415931, -3.047500000000091802 ) ) ;
#910 = LINE ( 'NONE', #246, #1515 ) ;
#911 = AXIS2_PLACEMENT_3D ( 'NONE', #3791, #7747, #7669 ) ;
#912 = DIRECTION ( 'NONE',  ( 1.000000000000000000, -3.549874073494553124E-30, 0.000000000000000000 ) ) ;
#913 = ORIENTED_EDGE ( 'NONE', *, *, #1158, .T. ) ;
#914 = CARTESIAN_POINT ( 'NONE',  ( 8.000000000000012434, -0.7805016046290649268, -6.776263578034402713E-15 ) ) ;
#915 = ORIENTED_EDGE ( 'NONE', *, *, #4440, .T. ) ;
#916 = EDGE_CURVE ( 'NONE', #8164, #6788, #3099, .T. ) ;
#917 = CARTESIAN_POINT ( 'NONE',  ( -8.000000000000007105, 3.871967595402132645, -0.4989386132324617473 ) ) ;
#918 = DIRECTION ( 'NONE',  ( -1.000000000000000000, 3.549874073494553124E-30, 0.000000000000000000 ) ) ;
#919 = CARTESIAN_POINT ( 'NONE',  ( 6.927742606685938292E-59, 3.903092032707603785E-29, -7.000000000000000888 ) ) ;
#920 = ORIENTED_EDGE ( 'NONE', *, *, #3291, .T. ) ;
#921 = CARTESIAN_POINT ( 'NONE',  ( -7.345652830559441071, 4.996589667937682222, -7.903584543330798518 ) ) ;
#922 = VERTEX_POINT ( 'NONE', #6767 ) ;
#923 = ORIENTED_EDGE ( 'NONE', *, *, #1782, .F. ) ;
#924 = B_SPLINE_CURVE_WITH_KNOTS ( 'NONE', 3,
 ( #7808, #3236, #3155, #464, #3111, #8429, #4459, #7121 ),
 .UNSPECIFIED., .F., .F.,
 ( 4, 2, 2, 4 ),
 ( 0.004673709593152105407, 0.005837709341827623452, 0.007001709090503142364, 0.009329708587854177587 ),
 .UNSPECIFIED. ) ;
#925 = CARTESIAN_POINT ( 'NONE',  ( -5.080504117408890075, -2.106769544347818712, -8.400000000000018119 ) ) ;
#926 = CARTESIAN_POINT ( 'NONE',  ( 0.6543471694414046969, 8.859816792613671055, -7.903584543331200862 ) ) ;
#927 = VERTEX_POINT ( 'NONE', #4267 ) ;
#928 = ADVANCED_FACE ( 'NONE', ( #1563 ), #213, .T. ) ;
#929 = DIRECTION ( 'NONE',  ( 0.000000000000000000, -0.000000000000000000, 1.000000000000000000 ) ) ;
#930 = EDGE_CURVE ( 'NONE', #462, #4330, #30, .T. ) ;
#931 = CIRCLE ( 'NONE', #2743, 8.000000000000007105 ) ;
#932 = LINE ( 'NONE', #892, #3752 ) ;
#933 = CARTESIAN_POINT ( 'NONE',  ( 350.0000000000000568, -1.249000902703301108E-13, -50.00000000000001421 ) ) ;
#934 = ORIENTED_EDGE ( 'NONE', *, *, #8009, .T. ) ;
#935 = CARTESIAN_POINT ( 'NONE',  ( 139.9999999999994316, 3.525609254162515373E-14, -4.172000000001442999 ) ) ;
#936 = EDGE_LOOP ( 'NONE', ( #4047, #6895, #1027, #2165 ) ) ;
#937 = FACE_OUTER_BOUND ( 'NONE', #8273, .T. ) ;
#938 = CARTESIAN_POINT ( 'NONE',  ( -45.49999999999950262, 152.5000000000003126, -1.942890293094023693E-13 ) ) ;
#939 = CARTESIAN_POINT ( 'NONE',  ( 0.000000000000000000, -3.469446951953614189E-15, 130.0000000000000000 ) ) ;
#940 = ORIENTED_EDGE ( 'NONE', *, *, #515, .F. ) ;
#941 = VECTOR ( 'NONE', #8021, 1000.000000000000000 ) ;
#942 = CARTESIAN_POINT ( 'NONE',  ( 10.00000000000000888, -650.0000000000002274, 79.99999999999995737 ) ) ;
#943 = EDGE_CURVE ( 'NONE', #4339, #7532, #6205, .T. ) ;
#944 = PRODUCT_DEFINITION ( 'UNKNOWN', '', #5930, #3848 ) ;
#945 =( LENGTH_UNIT ( ) NAMED_UNIT ( * ) SI_UNIT ( .MILLI., .METRE. ) );
#946 = ORIENTED_EDGE ( 'NONE', *, *, #5359, .T. ) ;
#947 = VERTEX_POINT ( 'NONE', #6980 ) ;
#948 = CARTESIAN_POINT ( 'NONE',  ( -8.000000000000007105, -4.618802153517065356, -0.7145311798163467287 ) ) ;
#949 = DIRECTION ( 'NONE',  ( 4.141519752410311978E-30, 8.626909098572831859E-16, 1.000000000000000000 ) ) ;
#950 = DIRECTION ( 'NONE',  ( 1.000000000000000000, 0.000000000000000000, 0.000000000000000000 ) ) ;
#951 = CARTESIAN_POINT ( 'NONE',  ( -3.999999999999781508, -6.928203230275875590, -8.400000000000018119 ) ) ;
#952 = EDGE_CURVE ( 'NONE', #2264, #484, #8525, .T. ) ;
#953 = DIRECTION ( 'NONE',  ( 0.000000000000000000, 1.064348848528640405E-29, -1.000000000000000000 ) ) ;
#954 = ORIENTED_EDGE ( 'NONE', *, *, #8456, .T. ) ;
#955 = CARTESIAN_POINT ( 'NONE',  ( 3.319543390096007407, -7.321065037175497281, -0.01688885742779770716 ) ) ;
#956 = ORIENTED_EDGE ( 'NONE', *, *, #7414, .F. ) ;
#957 = CARTESIAN_POINT ( 'NONE',  ( 0.000000000000000000, -299.9999999999999432, 75.00000000000002842 ) ) ;
#958 = EDGE_LOOP ( 'NONE', ( #3855, #811 ) ) ;
#959 = CIRCLE ( 'NONE', #5553, 15.00000000000000355 ) ;
#960 = B_SPLINE_CURVE_WITH_KNOTS ( 'NONE', 3,
 ( #5535, #4347, #4912, #5583, #7489, #247 ),
 .UNSPECIFIED., .F., .F.,
 ( 4, 2, 4 ),
 ( 0.008240550023493567466, 0.01057684187039396699, 0.01291313371729436651 ),
 .UNSPECIFIED. ) ;
#961 = CARTESIAN_POINT ( 'NONE',  ( 0.000000000000000000, 0.000000000000000000, 0.000000000000000000 ) ) ;
#962 = ORIENTED_EDGE ( 'NONE', *, *, #796, .T. ) ;
#963 = AXIS2_PLACEMENT_3D ( 'NONE', #1511, #3656, #291 ) ;
#964 = EDGE_CURVE ( 'NONE', #7587, #6592, #5196, .T. ) ;
#965 = ORIENTED_EDGE ( 'NONE', *, *, #7447, .T. ) ;
#966 = VECTOR ( 'NONE', #3191, 1000.000000000000000 ) ;
#967 = FACE_OUTER_BOUND ( 'NONE', #6917, .T. ) ;
#968 = DIRECTION ( 'NONE',  ( -7.703719777548943412E-34, 0.000000000000000000, 1.000000000000000000 ) ) ;
#969 = CARTESIAN_POINT ( 'NONE',  ( 3.318518101603053161, 7.321656987762952262, -8.399999999999966604 ) ) ;
#970 = CARTESIAN_POINT ( 'NONE',  ( -28.24999999999997513, 3.989921841591238568E-15, 18.00000000000000355 ) ) ;
#971 = ORIENTED_EDGE ( 'NONE', *, *, #6812, .T. ) ;
#972 = EDGE_CURVE ( 'NONE', #1241, #5649, #1680, .T. ) ;
#973 = CIRCLE ( 'NONE', #8341, 8.000000000000007105 ) ;
#974 = FACE_OUTER_BOUND ( 'NONE', #4758, .T. ) ;
#975 = CARTESIAN_POINT ( 'NONE',  ( 275.0000000000000000, -425.0000000000000000, 80.00000000000000000 ) ) ;
#976 = DIRECTION ( 'NONE',  ( 0.7235233670772677206, 0.6902998893909613187, 0.000000000000000000 ) ) ;
#977 = ORIENTED_EDGE ( 'NONE', *, *, #5273, .T. ) ;
#978 = DIRECTION ( 'NONE',  ( 1.034996974062501909E-32, -0.7071067811865503483, -0.7071067811865446862 ) ) ;
#979 = AXIS2_PLACEMENT_3D ( 'NONE', #2979, #8205, #1025 ) ;
#980 = CIRCLE ( 'NONE', #3190, 24.49999999999999645 ) ;
#981 = AXIS2_PLACEMENT_3D ( 'NONE', #6340, #5095, #364 ) ;
#982 = VERTEX_POINT ( 'NONE', #1520 ) ;
#983 = DIRECTION ( 'NONE',  ( 0.000000000000000000, 0.000000000000000000, 1.000000000000000000 ) ) ;
#984 = AXIS2_PLACEMENT_3D ( 'NONE', #3097, #5790, #2658 ) ;
#985 = EDGE_CURVE ( 'NONE', #2467, #3965, #3106, .T. ) ;
#986 = AXIS2_PLACEMENT_3D ( 'NONE', #223, #2880, #5550 ) ;
#987 = CARTESIAN_POINT ( 'NONE',  ( -6.661338147750939243E-13, -9.237604307034352757, -0.7145311798163467287 ) ) ;
#988 = VERTEX_POINT ( 'NONE', #6160 ) ;
#989 = VECTOR ( 'NONE', #3365, 1000.000000000000000 ) ;
#990 = CARTESIAN_POINT ( 'NONE',  ( 8.000000000000007105, 0.000000000000000000, 0.000000000000000000 ) ) ;
#991 =( NAMED_UNIT ( * ) SI_UNIT ( $, .STERADIAN. ) SOLID_ANGLE_UNIT ( ) );
#992 = ORIENTED_EDGE ( 'NONE', *, *, #3308, .F. ) ;
#993 = CIRCLE ( 'NONE', #5875, 8.000000000000007105 ) ;
#994 = PLANE ( 'NONE',  #6434 ) ;
#995 = EDGE_LOOP ( 'NONE', ( #6771, #4135, #161 ) ) ;
#996 = ORIENTED_EDGE ( 'NONE', *, *, #6739, .T. ) ;
#997 = CARTESIAN_POINT ( 'NONE',  ( 8.000000000000007105, 2.775557561562891351E-14, 6.661338147750939243E-13 ) ) ;
#998 = FACE_OUTER_BOUND ( 'NONE', #936, .T. ) ;
#999 = FACE_OUTER_BOUND ( 'NONE', #2827, .T. ) ;
#1000 = DIRECTION ( 'NONE',  ( -3.919652622816902408E-30, -3.944304526105059027E-30, 1.000000000000000000 ) ) ;
#1001 = CARTESIAN_POINT ( 'NONE',  ( 0.000000000000000000, 4.685197434473812983, 0.000000000000000000 ) ) ;
#1002 = CARTESIAN_POINT ( 'NONE',  ( 4.000000000000003553, -1.759474945355339992, -3.047499999999869758 ) ) ;
#1003 = LINE ( 'NONE', #6324, #6738 ) ;
#1004 = ORIENTED_EDGE ( 'NONE', *, *, #1173, .T. ) ;
#1005 = PLANE ( 'NONE',  #2797 ) ;
#1006 = EDGE_LOOP ( 'NONE', ( #2429, #302, #624, #3207, #7185, #3525, #718, #4684 ) ) ;
#1007 = EDGE_CURVE ( 'NONE', #4173, #282, #299, .T. ) ;
#1008 = CARTESIAN_POINT ( 'NONE',  ( 5.000000000000004441, -4.685197434473812095, 0.000000000000000000 ) ) ;
#1009 = DIRECTION ( 'NONE',  ( -1.000000000000000000, 3.549874073494553124E-30, 0.000000000000000000 ) ) ;
#1010 = EDGE_LOOP ( 'NONE', ( #4904, #534, #140, #1394 ) ) ;
#1011 = ORIENTED_EDGE ( 'NONE', *, *, #5241, .F. ) ;
#1012 = B_SPLINE_CURVE_WITH_KNOTS ( 'NONE', 3,
 ( #2126, #926, #1610, #4274, #969, #2969 ),
 .UNSPECIFIED., .F., .F.,
 ( 4, 2, 4 ),
 ( 2.380731633597212072E-07, 0.002336973833157672195, 0.004673709593151984844 ),
 .UNSPECIFIED. ) ;
#1013 = VECTOR ( 'NONE', #3964, 1000.000000000000000 ) ;
#1014 = ADVANCED_FACE ( 'NONE', ( #835 ), #3488, .F. ) ;
#1015 = EDGE_CURVE ( 'NONE', #8125, #3237, #183, .T. ) ;
#1016 = CIRCLE ( 'NONE', #3515, 8.000000000000007105 ) ;
#1017 = SURFACE_STYLE_USAGE ( .BOTH. , #2309 ) ;
#1018 = FACE_OUTER_BOUND ( 'NONE', #6088, .T. ) ;
#1019 = CARTESIAN_POINT ( 'NONE',  ( 6.689127551061982757, 5.375634714784596646, -0.3173508448886342426 ) ) ;
#1020 = ORIENTED_EDGE ( 'NONE', *, *, #2966, .T. ) ;
#1021 = CIRCLE ( 'NONE', #7137, 3.047499999999999876 ) ;
#1022 = DIRECTION ( 'NONE',  ( -6.938893903907228378E-17, 0.000000000000000000, -1.000000000000000000 ) ) ;
#1023 =( NAMED_UNIT ( * ) SI_UNIT ( $, .STERADIAN. ) SOLID_ANGLE_UNIT ( ) );
#1024 = ORIENTED_EDGE ( 'NONE', *, *, #7065, .T. ) ;
#1025 = DIRECTION ( 'NONE',  ( 1.000000000000000000, 0.000000000000000000, 0.000000000000000000 ) ) ;
#1026 = AXIS2_PLACEMENT_3D ( 'NONE', #1779, #2283, #6452 ) ;
#1027 = ORIENTED_EDGE ( 'NONE', *, *, #144, .T. ) ;
#1028 = DIRECTION ( 'NONE',  ( 6.400024471207000214E-36, -1.000000000000000000, 0.000000000000000000 ) ) ;
#1029 = ADVANCED_FACE ( 'NONE', ( #8280, #2872 ), #5541, .T. ) ;
#1030 = APPLICATION_CONTEXT ( 'automotive_design' ) ;
#1031 = FACE_OUTER_BOUND ( 'NONE', #1567, .T. ) ;
#1032 = EDGE_LOOP ( 'NONE', ( #1487, #8169 ) ) ;
#1033 = PLANE ( 'NONE',  #1948 ) ;
#1034 = ORIENTED_EDGE ( 'NONE', *, *, #6568, .F. ) ;
#1035 = B_SPLINE_CURVE_WITH_KNOTS ( 'NONE', 3,
 ( #4450, #8453, #2403, #2314, #7756, #2444, #6943, #2484 ),
 .UNSPECIFIED., .F., .F.,
 ( 4, 2, 2, 4 ),
 ( 0.004673709593152262400, 0.005837709341827771771, 0.007001709090503281142, 0.009329708587854299018 ),
 .UNSPECIFIED. ) ;
#1036 = B_SPLINE_CURVE_WITH_KNOTS ( 'NONE', 3,
 ( #7295, #1327, #3983, #5385, #808, #2239 ),
 .UNSPECIFIED., .F., .F.,
 ( 4, 2, 4 ),
 ( 2.380731626893816357E-07, 0.002336973833157379027, 0.004673709593152068111 ),
 .UNSPECIFIED. ) ;
#1037 = ORIENTED_EDGE ( 'NONE', *, *, #5557, .T. ) ;
#1038 = EDGE_LOOP ( 'NONE', ( #6111, #1879 ) ) ;
#1039 = LINE ( 'NONE', #6358, #7132 ) ;
#1040 = DIRECTION ( 'NONE',  ( -1.000000000000000000, 3.549874073494553124E-30, 0.000000000000000000 ) ) ;
#1041 = CARTESIAN_POINT ( 'NONE',  ( 50.00000000000004263, -500.0000000000000000, -45.00000000000000711 ) ) ;
#1042 = FACE_OUTER_BOUND ( 'NONE', #170, .T. ) ;
#1043 = CARTESIAN_POINT ( 'NONE',  ( -5.499999999999999112, 60.00000000000000000, -45.00000000000000711 ) ) ;
#1044 = DIRECTION ( 'NONE',  ( -1.000000000000000000, -8.881784197001244435E-16, -0.000000000000000000 ) ) ;
#1045 = ORIENTED_EDGE ( 'NONE', *, *, #8248, .T. ) ;
#1046 = EDGE_CURVE ( 'NONE', #7133, #5698, #2303, .T. ) ;
#1047 = PLANE ( 'NONE',  #561 ) ;
#1048 = ORIENTED_EDGE ( 'NONE', *, *, #2437, .F. ) ;
#1049 = AXIS2_PLACEMENT_3D ( 'NONE', #568, #2008, #5866 ) ;
#1050 = PRODUCT ( 'hex nut style 1_am_B18.2.4.1M - Hex nut, Style 1,  M10 x 1.5, with 16mm WAF --D-N', 'hex nut style 1_am_B18.2.4.1M - Hex nut, Style 1,  M10 x 1.5, with 16mm WAF --D-N', '', ( #2446 ) ) ;
#1051 = CARTESIAN_POINT ( 'NONE',  ( 0.000000000000000000, 0.000000000000000000, -8.400000000000018119 ) ) ;
#1052 = AXIS2_PLACEMENT_3D ( 'NONE', #2524, #6525, #3174 ) ;
#1053 = CONTEXT_DEPENDENT_SHAPE_REPRESENTATION ( #6091, #4806 ) ;
#1054 = CARTESIAN_POINT ( 'NONE',  ( 7.999999999999563016, -4.618802153517398423, -8.400000000000018119 ) ) ;
#1055 = VERTEX_POINT ( 'NONE', #4228 ) ;
#1056 = DIRECTION ( 'NONE',  ( -0.000000000000000000, -0.000000000000000000, 1.000000000000000000 ) ) ;
#1057 = ADVANCED_FACE ( 'NONE', ( #6242 ), #5780, .T. ) ;
#1058 = LINE ( 'NONE', #6898, #8106 ) ;
#1059 = FACE_OUTER_BOUND ( 'NONE', #3912, .T. ) ;
#1060 = ORIENTED_EDGE ( 'NONE', *, *, #5786, .F. ) ;
#1061 = CARTESIAN_POINT ( 'NONE',  ( 15.50000000000011191, -14.99999999999990230, 79.99999999999995737 ) ) ;
#1062 = EDGE_CURVE ( 'NONE', #828, #3789, #4177, .T. ) ;
#1063 = CARTESIAN_POINT ( 'NONE',  ( 0.000000000000000000, 0.000000000000000000, 0.000000000000000000 ) ) ;
#1064 = APPLICATION_PROTOCOL_DEFINITION ( 'draft international standard', 'automotive_design', 1998, #1468 ) ;
#1065 = CIRCLE ( 'NONE', #7877, 5.700000000000001954 ) ;
#1066 = FACE_BOUND ( 'NONE', #7624, .T. ) ;
#1067 = LINE ( 'NONE', #4415, #4716 ) ;
#1068 = VERTEX_POINT ( 'NONE', #919 ) ;
#1069 = DIRECTION ( 'NONE',  ( 1.000000000000000000, -1.774937036747276562E-30, -9.447016907875728896E-60 ) ) ;
#1070 = EDGE_CURVE ( 'NONE', #8094, #5152, #5051, .T. ) ;
#1071 = VERTEX_POINT ( 'NONE', #8236 ) ;
#1072 = DIRECTION ( 'NONE',  ( 0.000000000000000000, 0.000000000000000000, -1.000000000000000000 ) ) ;
#1073 = ORIENTED_EDGE ( 'NONE', *, *, #5836, .F. ) ;
#1074 = DIRECTION ( 'NONE',  ( -1.000000000000000000, 3.549874073494553124E-30, 0.000000000000000000 ) ) ;
#1075 = CONICAL_SURFACE ( 'NONE', #8033, 8.000000000000007105, 1.047197551196597631 ) ;
#1076 = CARTESIAN_POINT ( 'NONE',  ( 4.000000000000003553, 6.928203230275431501, -8.400000000000018119 ) ) ;
#1077 = ADVANCED_FACE ( 'NONE', ( #2263 ), #4920, .T. ) ;
#1078 = PLANE ( 'NONE',  #3345 ) ;
#1079 = CARTESIAN_POINT ( 'NONE',  ( -0.6543471694415553541, -8.859816792613555592, -0.4964154566687579706 ) ) ;
#1080 = ADVANCED_FACE ( 'NONE', ( #3746 ), #5169, .F. ) ;
#1081 = CARTESIAN_POINT ( 'NONE',  ( 4.000000000000058620, 3.518949890710762585, 2.220446049250313081E-13 ) ) ;
#1082 = EDGE_LOOP ( 'NONE', ( #5118, #7351, #210 ) ) ;
#1083 = CARTESIAN_POINT ( 'NONE',  ( 8.000000000000007105, 0.000000000000000000, 0.000000000000000000 ) ) ;
#1084 = ORIENTED_EDGE ( 'NONE', *, *, #254, .T. ) ;
#1085 = DIRECTION ( 'NONE',  ( 6.400024471206996205E-36, -1.000000000000000000, -7.598173571352216173E-18 ) ) ;
#1086 = ITEM_DEFINED_TRANSFORMATION ( 'NONE', 'NONE', #6062,  #7563 ) ;
#1087 = CARTESIAN_POINT ( 'NONE',  ( 5.000000000000115463, -14.99999999999990230, 0.000000000000000000 ) ) ;
#1088 = EDGE_LOOP ( 'NONE', ( #2286, #7303, #3156, #836 ) ) ;
#1089 = EDGE_LOOP ( 'NONE', ( #1523, #8174, #4178, #8253, #3250 ) ) ;
#1090 = PLANE ( 'NONE',  #1105 ) ;
#1091 = VECTOR ( 'NONE', #8406, 1000.000000000000000 ) ;
#1092 = CARTESIAN_POINT ( 'NONE',  ( 33.00000000000055422, -1.431146867680865853E-14, 6.883382752675970551E-12 ) ) ;
#1093 = CARTESIAN_POINT ( 'NONE',  ( 5.000000000000004441, 0.000000000000000000, 0.000000000000000000 ) ) ;
#1094 = CARTESIAN_POINT ( 'NONE',  ( 0.000000000000000000, 0.000000000000000000, -8.400000000000018119 ) ) ;
#1095 = ORIENTED_EDGE ( 'NONE', *, *, #386, .F. ) ;
#1096 = DIRECTION ( 'NONE',  ( -1.463706757734299248E-32, 1.000000000000000000, 5.238529448733281520E-32 ) ) ;
#1097 = CARTESIAN_POINT ( 'NONE',  ( -4.440892098500626162E-13, -9.237604307034018802, -7.685468820183672278 ) ) ;
#1098 = DIRECTION ( 'NONE',  ( 1.000000000000000000, 8.736544766236848795E-16, -1.058471975245254351E-16 ) ) ;
#1099 = CARTESIAN_POINT ( 'NONE',  ( -5.354491962338076227, 6.146186931204334236, -8.331901280394644616 ) ) ;
#1100 = EDGE_CURVE ( 'NONE', #6142, #92, #6057, .T. ) ;
#1101 = AXIS2_PLACEMENT_3D ( 'NONE', #2723, #668, #4640 ) ;
#1102 = DIRECTION ( 'NONE',  ( 0.000000000000000000, 0.000000000000000000, 1.000000000000000000 ) ) ;
#1103 = ORIENTED_EDGE ( 'NONE', *, *, #2966, .F. ) ;
#1104 = CARTESIAN_POINT ( 'NONE',  ( -49.99999999999963762, 87.50000000000035527, 9.999999999999786837 ) ) ;
#1105 = AXIS2_PLACEMENT_3D ( 'NONE', #1685, #4478, #520 ) ;
#1106 = ORIENTED_EDGE ( 'NONE', *, *, #8367, .F. ) ;
#1107 = CARTESIAN_POINT ( 'NONE',  ( -25.74999999999981526, 15.00000000000010836, 10.00000000000000888 ) ) ;
#1108 = ORIENTED_EDGE ( 'NONE', *, *, #2386, .T. ) ;
#1109 = DIRECTION ( 'NONE',  ( -0.5000000000000033307, -0.8660254037844367092, 0.000000000000000000 ) ) ;
#1110 = ADVANCED_FACE ( 'NONE', ( #7138 ), #5042, .F. ) ;
#1111 = CLOSED_SHELL ( 'NONE', ( #1558, #3745, #5880, #1315, #2465, #1923, #2389, #8392, #4690, #2185, #2012, #7267, #3909, #5796, #8296, #154, #7284, #6547, #2936, #1396, #8597, #759 ) ) ;
#1112 = ADVANCED_FACE ( 'NONE', ( #7873 ), #2726, .T. ) ;
#1113 = VECTOR ( 'NONE', #7329, 1000.000000000000000 ) ;
#1114 = LINE ( 'NONE', #467, #1443 ) ;
#1115 = DIRECTION ( 'NONE',  ( 0.000000000000000000, 0.000000000000000000, 1.000000000000000000 ) ) ;
#1116 = PRESENTATION_STYLE_ASSIGNMENT (( #3120 ) ) ;
#1117 = CARTESIAN_POINT ( 'NONE',  ( 10.00000000000001599, 2.945121478342286219E-29, -5.399999999999590905 ) ) ;
#1118 = CIRCLE ( 'NONE', #8079, 10.00000000000000178 ) ;
#1119 = DIRECTION ( 'NONE',  ( 3.919652622816902408E-30, 3.944304526105059027E-30, -1.000000000000000000 ) ) ;
#1120 = CARTESIAN_POINT ( 'NONE',  ( 3.659266894335830776E-32, -299.9999999999999432, 69.99999999999992895 ) ) ;
#1121 = DIRECTION ( 'NONE',  ( 0.000000000000000000, -1.000000000000000000, -1.795949010423047620E-16 ) ) ;
#1122 = EDGE_LOOP ( 'NONE', ( #2153, #1445, #329, #3321 ) ) ;
#1123 = ORIENTED_EDGE ( 'NONE', *, *, #5960, .F. ) ;
#1124 = EDGE_CURVE ( 'NONE', #8386, #828, #1181, .T. ) ;
#1125 = DIRECTION ( 'NONE',  ( -1.000000000000000000, 0.000000000000000000, 0.000000000000000000 ) ) ;
#1126 = ITEM_DEFINED_TRANSFORMATION ( 'NONE', 'NONE', #5347,  #7563 ) ;
#1127 = DIRECTION ( 'NONE',  ( 2.842664852890546338E-35, -1.000000000000000000, 0.000000000000000000 ) ) ;
#1128 = ORIENTED_EDGE ( 'NONE', *, *, #2618, .F. ) ;
#1129 = ORIENTED_EDGE ( 'NONE', *, *, #6644, .F. ) ;
#1130 = CARTESIAN_POINT ( 'NONE',  ( -86.99999999999943157, 120.0000000000003126, -2.775557561562893244E-14 ) ) ;
#1131 = EDGE_CURVE ( 'NONE', #5665, #6135, #2302, .T. ) ;
#1132 = UNCERTAINTY_MEASURE_WITH_UNIT (LENGTH_MEASURE( 1.000000000000000082E-05 ), #1546, 'distance_accuracy_value', 'NONE');
#1133 = FACE_BOUND ( 'NONE', #2656, .T. ) ;
#1134 = DIRECTION ( 'NONE',  ( 0.8660254037844369313, 0.5000000000000028866, 0.000000000000000000 ) ) ;
#1135 = ORIENTED_EDGE ( 'NONE', *, *, #343, .T. ) ;
#1136 = DIRECTION ( 'NONE',  ( 1.000000000000000000, -1.774937036747276562E-30, -9.447016907875728896E-60 ) ) ;
#1137 = DIRECTION ( 'NONE',  ( 0.000000000000000000, 0.000000000000000000, 1.000000000000000000 ) ) ;
#1138 = DIRECTION ( 'NONE',  ( 0.000000000000000000, 0.000000000000000000, -1.000000000000000000 ) ) ;
#1139 = APPLICATION_PROTOCOL_DEFINITION ( 'draft international standard', 'automotive_design', 1998, #6645 ) ;
#1140 = AXIS2_PLACEMENT_3D ( 'NONE', #6510, #5843, #8469 ) ;
#1141 = AXIS2_PLACEMENT_3D ( 'NONE', #4803, #4838, #2838 ) ;
#1142 = CARTESIAN_POINT ( 'NONE',  ( 5.080504117408890075, 2.106769544347818268, 5.551115123125782702E-14 ) ) ;
#1143 = ORIENTED_EDGE ( 'NONE', *, *, #1936, .T. ) ;
#1144 = DIRECTION ( 'NONE',  ( -1.463706757734299248E-32, 1.000000000000000000, 5.238529448733281520E-32 ) ) ;
#1145 = AXIS2_PLACEMENT_3D ( 'NONE', #2007, #3490, #6118 ) ;
#1146 = DIRECTION ( 'NONE',  ( -0.000000000000000000, -0.000000000000000000, 1.000000000000000000 ) ) ;
#1147 = EDGE_LOOP ( 'NONE', ( #2427, #2249, #1617 ) ) ;
#1148 = EDGE_CURVE ( 'NONE', #7803, #3139, #2994, .T. ) ;
#1149 = CARTESIAN_POINT ( 'NONE',  ( -15.00000000000002487, 1.926036882627243013E-34, 18.00000000000000355 ) ) ;
#1150 = ORIENTED_EDGE ( 'NONE', *, *, #5995, .F. ) ;
#1151 = LINE ( 'NONE', #334, #6858 ) ;
#1152 = UNCERTAINTY_MEASURE_WITH_UNIT (LENGTH_MEASURE( 1.000000000000000082E-05 ), #5243, 'distance_accuracy_value', 'NONE');
#1153 = AXIS2_PLACEMENT_3D ( 'NONE', #6835, #864, #4865 ) ;
#1154 = CARTESIAN_POINT ( 'NONE',  ( 5.000000000000004441, -2.159584836538827029E-29, 4.057500000000000107 ) ) ;
#1155 = FACE_OUTER_BOUND ( 'NONE', #817, .T. ) ;
#1156 = CARTESIAN_POINT ( 'NONE',  ( -0.6543471694412575923, -8.859816792613658620, -0.4964154566688018799 ) ) ;
#1157 = CARTESIAN_POINT ( 'NONE',  ( -45.49999999999963052, 87.50000000000036948, 9.999999999999786837 ) ) ;
#1158 = EDGE_CURVE ( 'NONE', #799, #2305, #2606, .T. ) ;
#1159 = CARTESIAN_POINT ( 'NONE',  ( 5.354491962337593947, -6.146186931204438153, -0.06809871960523644630 ) ) ;
#1160 = EDGE_LOOP ( 'NONE', ( #4751, #8064 ) ) ;
#1161 = EDGE_CURVE ( 'NONE', #2145, #4173, #4390, .T. ) ;
#1162 = ORIENTED_EDGE ( 'NONE', *, *, #899, .F. ) ;
#1163 = AXIS2_PLACEMENT_3D ( 'NONE', #8403, #4472, #516 ) ;
#1164 = AXIS2_PLACEMENT_3D ( 'NONE', #4149, #7550, #1616 ) ;
#1165 = CARTESIAN_POINT ( 'NONE',  ( 3.318518101602791148, 7.321656987762752422, 1.179340913121107448E-13 ) ) ;
#1166 = DIRECTION ( 'NONE',  ( -0.000000000000000000, -1.000000000000000000, -0.000000000000000000 ) ) ;
#1167 = ORIENTED_EDGE ( 'NONE', *, *, #2419, .F. ) ;
#1168 = FACE_OUTER_BOUND ( 'NONE', #1171, .T. ) ;
#1169 = ORIENTED_EDGE ( 'NONE', *, *, #5273, .F. ) ;
#1170 = ADVANCED_FACE ( 'NONE', ( #3127 ), #3214, .F. ) ;
#1171 = EDGE_LOOP ( 'NONE', ( #804, #4109, #3770, #257 ) ) ;
#1172 = DIRECTION ( 'NONE',  ( 1.463706757734299248E-32, -1.000000000000000000, 4.930380657631321594E-32 ) ) ;
#1173 = EDGE_CURVE ( 'NONE', #3827, #1071, #355, .T. ) ;
#1174 = CARTESIAN_POINT ( 'NONE',  ( -4.440892098500626162E-13, -9.237604307034018802, -0.7145311798163467287 ) ) ;
#1175 = LINE ( 'NONE', #6489, #2104 ) ;
#1176 = ORIENTED_EDGE ( 'NONE', *, *, #245, .T. ) ;
#1177 = LINE ( 'NONE', #1828, #3923 ) ;
#1178 = CARTESIAN_POINT ( 'NONE',  ( -0.6527133886637680460, 8.860760056386036254, -7.903039949738070113 ) ) ;
#1179 = PRODUCT ( 'socket head cap screw_am_B18.3.1M - 8 x 1.25 x 25 Hex SHCS -- 25NHX', 'socket head cap screw_am_B18.3.1M - 8 x 1.25 x 25 Hex SHCS -- 25NHX', '', ( #1697 ) ) ;
#1180 = CARTESIAN_POINT ( 'NONE',  ( 2.644994884458577555, -7.710515798486396122, -8.317753204360382568 ) ) ;
#1181 = CIRCLE ( 'NONE', #6081, 80.00000000000001421 ) ;
#1182 = LINE ( 'NONE', #3360, #5916 ) ;
#1183 = EDGE_LOOP ( 'NONE', ( #5544, #5968 ) ) ;
#1184 = B_SPLINE_CURVE_WITH_KNOTS ( 'NONE', 3,
 ( #606, #1997, #16, #3959, #111, #5450, #4660, #5398 ),
 .UNSPECIFIED., .F., .F.,
 ( 4, 2, 2, 4 ),
 ( 0.004673709593152015201, 0.005837709341827572278, 0.007001709090503129354, 0.009329708587854243507 ),
 .UNSPECIFIED. ) ;
#1185 = CARTESIAN_POINT ( 'NONE',  ( 8.000000000000117240, 4.618802153516954334, -8.400000000000018119 ) ) ;
#1186 = ORIENTED_EDGE ( 'NONE', *, *, #2194, .F. ) ;
#1187 = DIRECTION ( 'NONE',  ( -0.000000000000000000, -0.000000000000000000, 1.000000000000000000 ) ) ;
#1188 = ORIENTED_EDGE ( 'NONE', *, *, #7824, .F. ) ;
#1189 = DIRECTION ( 'NONE',  ( -3.451266460341926211E-31, 0.4999999999999985567, -0.8660254037844393737 ) ) ;
#1190 = EDGE_CURVE ( 'NONE', #6484, #5439, #6552, .T. ) ;
#1191 = CARTESIAN_POINT ( 'NONE',  ( 0.000000000000000000, 0.000000000000000000, 0.000000000000000000 ) ) ;
#1192 = PRODUCT_RELATED_PRODUCT_CATEGORY ( 'part', '', ( #3195 ) ) ;
#1193 = VECTOR ( 'NONE', #3510, 1000.000000000000000 ) ;
#1194 = CARTESIAN_POINT ( 'NONE',  ( -49.99999999999949551, 152.5000000000003126, -1.942890293094023946E-13 ) ) ;
#1195 = CARTESIAN_POINT ( 'NONE',  ( 8.000000000000008882, 1.572549600175702444, -0.06894455525514735228 ) ) ;
#1196 = CARTESIAN_POINT ( 'NONE',  ( 4.000000000000003553, 1.759474945355415931, -3.047500000000091802 ) ) ;
#1197 = DIRECTION ( 'NONE',  ( 1.619075244245011343E-15, 1.000000000000000000, -3.845696912952415736E-30 ) ) ;
#1198 = ORIENTED_EDGE ( 'NONE', *, *, #1015, .F. ) ;
#1199 = AXIS2_PLACEMENT_3D ( 'NONE', #4817, #4940, #4156 ) ;
#1200 = VERTEX_POINT ( 'NONE', #5219 ) ;
#1201 = CARTESIAN_POINT ( 'NONE',  ( 275.0000000000000000, 425.0000000000000000, 80.00000000000015632 ) ) ;
#1202 = DIRECTION ( 'NONE',  ( 0.000000000000000000, -5.908893405598423146E-30, 1.000000000000000000 ) ) ;
#1203 = DIRECTION ( 'NONE',  ( 1.000000000000000000, -0.000000000000000000, -6.938893903907228378E-17 ) ) ;
#1204 = ADVANCED_FACE ( 'NONE', ( #7784 ), #1471, .T. ) ;
#1205 = ITEM_DEFINED_TRANSFORMATION ( 'NONE', 'NONE', #2844,  #7563 ) ;
#1206 = ORIENTED_EDGE ( 'NONE', *, *, #795, .T. ) ;
#1207 = FACE_OUTER_BOUND ( 'NONE', #4849, .T. ) ;
#1208 = AXIS2_PLACEMENT_3D ( 'NONE', #2292, #4757, #7404 ) ;
#1209 = ORIENTED_EDGE ( 'NONE', *, *, #3887, .T. ) ;
#1210 = CARTESIAN_POINT ( 'NONE',  ( -3.999999999999781508, -6.928203230275875590, -8.400000000000018119 ) ) ;
#1211 = ORIENTED_EDGE ( 'NONE', *, *, #2083, .T. ) ;
#1212 = CARTESIAN_POINT ( 'NONE',  ( 4.000000000000003553, 1.759474945355374409, 3.047499999999869758 ) ) ;
#1213 = ORIENTED_EDGE ( 'NONE', *, *, #1949, .T. ) ;
#1214 = DIRECTION ( 'NONE',  ( 0.000000000000000000, 0.000000000000000000, 1.000000000000000000 ) ) ;
#1215 = DIRECTION ( 'NONE',  ( 0.000000000000000000, -1.042965139114318115E-29, 1.000000000000000000 ) ) ;
#1216 = EDGE_CURVE ( 'NONE', #982, #5776, #7594, .T. ) ;
#1217 = CARTESIAN_POINT ( 'NONE',  ( 8.000000000000117240, -1.110223024625156540E-13, 0.000000000000000000 ) ) ;
#1218 = CARTESIAN_POINT ( 'NONE',  ( -8.000000000000229150, 4.618802153516954334, -8.400000000000018119 ) ) ;
#1219 = VERTEX_POINT ( 'NONE', #440 ) ;
#1220 = CARTESIAN_POINT ( 'NONE',  ( -0.6543471694416780338, -8.859816792613822045, -7.903584543331102275 ) ) ;
#1221 = APPLICATION_PROTOCOL_DEFINITION ( 'draft international standard', 'automotive_design', 1998, #2802 ) ;
#1222 = EDGE_CURVE ( 'NONE', #7754, #1987, #70, .T. ) ;
#1223 = VERTEX_POINT ( 'NONE', #5770 ) ;
#1224 = CARTESIAN_POINT ( 'NONE',  ( 8.000000000000232703, 0.7809653281575155148, -8.399999999999890221 ) ) ;
#1225 =( NAMED_UNIT ( * ) SI_UNIT ( $, .STERADIAN. ) SOLID_ANGLE_UNIT ( ) );
#1226 = EDGE_LOOP ( 'NONE', ( #2572, #6026, #2747, #6490 ) ) ;
#1227 = EDGE_CURVE ( 'NONE', #4883, #4829, #1432, .T. ) ;
#1228 = CARTESIAN_POINT ( 'NONE',  ( 1.313474075707028232, 8.479269695850733868, -8.083279549040270240 ) ) ;
#1229 = VERTEX_POINT ( 'NONE', #2040 ) ;
#1230 = CARTESIAN_POINT ( 'NONE',  ( -5.690023276062465385, -5.952467836904175691, -0.1306530452038474899 ) ) ;
#1231 = B_SPLINE_CURVE_WITH_KNOTS ( 'NONE', 3,
 ( #6988, #7586, #1692, #6454, #2970, #1019, #4366, #1611 ),
 .UNSPECIFIED., .F., .F.,
 ( 4, 2, 2, 4 ),
 ( 0.004673709593152763735, 0.005837709341828114379, 0.007001709090503465890, 0.009329708587854167179 ),
 .UNSPECIFIED. ) ;
#1232 = ADVANCED_FACE ( 'NONE', ( #779, #7221 ), #4563, .F. ) ;
#1233 = VECTOR ( 'NONE', #2637, 999.9999999999998863 ) ;
#1234 = CARTESIAN_POINT ( 'NONE',  ( 2.644994884458959916, -7.710515798486509809, -8.317753204360252894 ) ) ;
#1235 = CIRCLE ( 'NONE', #129, 5.500000000000024869 ) ;
#1236 = CARTESIAN_POINT ( 'NONE',  ( 0.000000000000000000, 0.000000000000000000, 0.000000000000000000 ) ) ;
#1237 = CARTESIAN_POINT ( 'NONE',  ( 0.000000000000000000, 0.000000000000000000, -8.400000000000018119 ) ) ;
#1238 = DIRECTION ( 'NONE',  ( -0.000000000000000000, -0.000000000000000000, 1.000000000000000000 ) ) ;
#1239 = CARTESIAN_POINT ( 'NONE',  ( 8.000000000000007105, 0.000000000000000000, -8.400000000000018119 ) ) ;
#1240 = ORIENTED_EDGE ( 'NONE', *, *, #1158, .F. ) ;
#1241 = VERTEX_POINT ( 'NONE', #3296 ) ;
#1242 = PLANE ( 'NONE',  #6638 ) ;
#1243 = CLOSED_SHELL ( 'NONE', ( #5729, #3388, #3751, #716, #4098, #5564 ) ) ;
#1244 = AXIS2_PLACEMENT_3D ( 'NONE', #8165, #2850, #7552 ) ;
#1245 = CARTESIAN_POINT ( 'NONE',  ( -8.000000000000222045, -3.867591403079432055, -0.4976753153247615580 ) ) ;
#1246 = CARTESIAN_POINT ( 'NONE',  ( -8.000000000000117240, -1.110223024625156540E-13, -8.400000000000018119 ) ) ;
#1247 = CONICAL_SURFACE ( 'NONE', #6948, 8.000000000000007105, 1.047197551196597631 ) ;
#1248 = ORIENTED_EDGE ( 'NONE', *, *, #1592, .T. ) ;
#1249 = DIRECTION ( 'NONE',  ( 1.000000000000000000, 8.881784197001244435E-16, 0.000000000000000000 ) ) ;
#1250 = CIRCLE ( 'NONE', #4040, 8.000000000000007105 ) ;
#1251 = VERTEX_POINT ( 'NONE', #3437 ) ;
#1252 = ORIENTED_EDGE ( 'NONE', *, *, #6887, .F. ) ;
#1253 = VECTOR ( 'NONE', #5699, 1000.000000000000000 ) ;
#1254 = EDGE_CURVE ( 'NONE', #1438, #6198, #65, .T. ) ;
#1255 = FACE_OUTER_BOUND ( 'NONE', #4456, .T. ) ;
#1256 = ORIENTED_EDGE ( 'NONE', *, *, #8260, .T. ) ;
#1257 = CARTESIAN_POINT ( 'NONE',  ( -4.000000000000003553, 6.928203230275431501, -8.400000000000018119 ) ) ;
#1258 = LINE ( 'NONE', #1402, #6863 ) ;
#1259 = CARTESIAN_POINT ( 'NONE',  ( -8.000000000000007105, -4.618802153517398423, -7.685468820183672278 ) ) ;
#1260 = DIRECTION ( 'NONE',  ( 3.851859888774471706E-33, -7.598173571352223877E-18, 1.000000000000000000 ) ) ;
#1261 = DIRECTION ( 'NONE',  ( -1.000000000000000000, 1.774937036747276562E-30, 0.000000000000000000 ) ) ;
#1262 = CARTESIAN_POINT ( 'NONE',  ( -8.000000000000007105, 1.110223024625156540E-13, -8.400000000000018119 ) ) ;
#1263 = ORIENTED_EDGE ( 'NONE', *, *, #2548, .T. ) ;
#1264 = DIRECTION ( 'NONE',  ( -1.000000000000000000, 3.549874073494553124E-30, 3.778304382545602261E-59 ) ) ;
#1265 =( LENGTH_UNIT ( ) NAMED_UNIT ( * ) SI_UNIT ( .MILLI., .METRE. ) );
#1266 = EDGE_CURVE ( 'NONE', #8505, #6546, #8013, .T. ) ;
#1267 = ITEM_DEFINED_TRANSFORMATION ( 'NONE', 'NONE', #1164,  #7563 ) ;
#1268 = EDGE_CURVE ( 'NONE', #2856, #3046, #7904, .T. ) ;
#1269 = CARTESIAN_POINT ( 'NONE',  ( -5.080504117408896292, -2.106769544347821377, 0.000000000000000000 ) ) ;
#1270 = LINE ( 'NONE', #7327, #6124 ) ;
#1271 = ORIENTED_EDGE ( 'NONE', *, *, #7626, .T. ) ;
#1272 = CARTESIAN_POINT ( 'NONE',  ( -31.74999999999994316, -1.972152263052529514E-28, 0.000000000000000000 ) ) ;
#1273 = DIRECTION ( 'NONE',  ( 0.000000000000000000, 0.000000000000000000, 1.000000000000000000 ) ) ;
#1274 = ORIENTED_EDGE ( 'NONE', *, *, #6405, .T. ) ;
#1275 = CIRCLE ( 'NONE', #3368, 70.00000000000008527 ) ;
#1276 = ADVANCED_FACE ( 'NONE', ( #3343 ), #2439, .T. ) ;
#1277 = CIRCLE ( 'NONE', #4765, 24.50000000000000000 ) ;
#1278 = CIRCLE ( 'NONE', #4344, 5.500000000000024869 ) ;
#1279 = SHAPE_REPRESENTATION ( 'MAT-028', ( #4102, #8402, #6596, #2160, #7023, #1164, #4651, #481, #8132, #5347, #4373, #2844, #1583, #618, #5496, #7708, #3953, #6062, #752, #5647, #1861, #6746, #7842, #900, #339, #5200, #7577, #2288, #2010, #4801, #1870, #6601 ), #199 ) ;
#1280 = CARTESIAN_POINT ( 'NONE',  ( -34.92499999999998295, 0.000000000000000000, 0.000000000000000000 ) ) ;
#1281 = ORIENTED_EDGE ( 'NONE', *, *, #854, .F. ) ;
#1282 = CARTESIAN_POINT ( 'NONE',  ( -4.339467034331305761, -6.732211846623399332, -3.359396196281597955E-14 ) ) ;
#1283 = PLANE ( 'NONE',  #3713 ) ;
#1284 = CARTESIAN_POINT ( 'NONE',  ( 4.000000000000003553, 1.759474945355415931, -3.047500000000091802 ) ) ;
#1285 = DIRECTION ( 'NONE',  ( 6.400024471206996205E-36, -1.000000000000000000, -7.598173571352216173E-18 ) ) ;
#1286 = CARTESIAN_POINT ( 'NONE',  ( -275.0000000000000000, -425.0000000000000000, -75.00000000000000000 ) ) ;
#1287 = CARTESIAN_POINT ( 'NONE',  ( 0.000000000000000000, 0.000000000000000000, 0.000000000000000000 ) ) ;
#1288 = ORIENTED_EDGE ( 'NONE', *, *, #153, .F. ) ;
#1289 = VECTOR ( 'NONE', #8334, 1000.000000000000114 ) ;
#1290 = FACE_BOUND ( 'NONE', #1032, .T. ) ;
#1291 = ORIENTED_EDGE ( 'NONE', *, *, #5574, .F. ) ;
#1292 = CARTESIAN_POINT ( 'NONE',  ( 8.000000000000229150, 4.618802153516954334, -8.400000000000018119 ) ) ;
#1293 = AXIS2_PLACEMENT_3D ( 'NONE', #1876, #7191, #1215 ) ;
#1294 = EDGE_CURVE ( 'NONE', #7390, #3622, #2823, .T. ) ;
#1295 = CARTESIAN_POINT ( 'NONE',  ( 7.345652830558382362, -4.996589667937645807, -0.4964154566687026815 ) ) ;
#1296 = CARTESIAN_POINT ( 'NONE',  ( 8.000000000000234479, 3.115336682266935497, -0.3193931313916126280 ) ) ;
#1297 = VECTOR ( 'NONE', #4764, 1000.000000000000114 ) ;
#1298 = CARTESIAN_POINT ( 'NONE',  ( -7.345652830558729640, 4.996589667937282542, -0.4964154566687483117 ) ) ;
#1299 = VECTOR ( 'NONE', #5348, 1000.000000000000000 ) ;
#1300 =( REPRESENTATION_RELATIONSHIP ('NONE','NONE', #1279, #4603 ) REPRESENTATION_RELATIONSHIP_WITH_TRANSFORMATION ( #572 )SHAPE_REPRESENTATION_RELATIONSHIP( ) );
#1301 = ADVANCED_FACE ( 'NONE', ( #5308 ), #5261, .T. ) ;
#1302 = EDGE_CURVE ( 'NONE', #7833, #7189, #3565, .T. ) ;
#1303 = DIRECTION ( 'NONE',  ( 0.000000000000000000, 0.000000000000000000, -1.000000000000000000 ) ) ;
#1304 = ORIENTED_EDGE ( 'NONE', *, *, #8456, .F. ) ;
#1305 = ORIENTED_EDGE ( 'NONE', *, *, #108, .T. ) ;
#1306 = VECTOR ( 'NONE', #3279, 1000.000000000000000 ) ;
#1307 = AXIS2_PLACEMENT_3D ( 'NONE', #3854, #546, #3204 ) ;
#1308 = CARTESIAN_POINT ( 'NONE',  ( -2.220446049250313081E-13, -650.0000000000000000, -1.110223024625156540E-13 ) ) ;
#1309 = ORIENTED_EDGE ( 'NONE', *, *, #5469, .F. ) ;
#1310 = CARTESIAN_POINT ( 'NONE',  ( 0.000000000000000000, 4.685197434473812983, 0.000000000000000000 ) ) ;
#1311 = CARTESIAN_POINT ( 'NONE',  ( -2.309976723937750887, 7.903938623646893369, -0.1306530452038467960 ) ) ;
#1312 = FACE_BOUND ( 'NONE', #1183, .T. ) ;
#1313 = DIRECTION ( 'NONE',  ( 0.000000000000000000, 0.000000000000000000, 1.000000000000000000 ) ) ;
#1314 = LINE ( 'NONE', #1218, #3212 ) ;
#1315 = ADVANCED_FACE ( 'NONE', ( #7307 ), #1341, .F. ) ;
#1316 = ORIENTED_EDGE ( 'NONE', *, *, #7500, .T. ) ;
#1317 = DIRECTION ( 'NONE',  ( 1.000000000000000000, 3.083952846180992055E-15, 0.000000000000000000 ) ) ;
#1318 = ITEM_DEFINED_TRANSFORMATION ( 'NONE', 'NONE', #481,  #7563 ) ;
#1319 =( LENGTH_UNIT ( ) NAMED_UNIT ( * ) SI_UNIT ( .MILLI., .METRE. ) );
#1320 = DIRECTION ( 'NONE',  ( -6.938893903907228378E-17, 0.000000000000000000, -1.000000000000000000 ) ) ;
#1321 = EDGE_CURVE ( 'NONE', #4696, #7027, #2696, .T. ) ;
#1322 = ORIENTED_EDGE ( 'NONE', *, *, #3699, .F. ) ;
#1323 = CYLINDRICAL_SURFACE ( 'NONE', #4448, 4.499999999999990230 ) ;
#1324 = ORIENTED_EDGE ( 'NONE', *, *, #1689, .T. ) ;
#1325 = CARTESIAN_POINT ( 'NONE',  ( 50.00000000000004263, -500.0000000000000000, -50.00000000000000000 ) ) ;
#1326 = EDGE_LOOP ( 'NONE', ( #2945, #5668, #1084, #7460 ) ) ;
#1327 = CARTESIAN_POINT ( 'NONE',  ( 7.345652830558381474, -4.996589667937645807, -7.903584543331313661 ) ) ;
#1328 = EDGE_CURVE ( 'NONE', #828, #6748, #1386, .T. ) ;
#1329 = CARTESIAN_POINT ( 'NONE',  ( 0.6527133886625517967, -8.860760056386085992, -7.903039949738097647 ) ) ;
#1330 = EDGE_CURVE ( 'NONE', #530, #3192, #731, .T. ) ;
#1331 = CARTESIAN_POINT ( 'NONE',  ( 3.000384657911015074E-15, -299.9999999999999432, -24.50000000000002487 ) ) ;
#1332 = CARTESIAN_POINT ( 'NONE',  ( -50.00000000000004263, -425.0000000000000000, 3.469446951953614189E-15 ) ) ;
#1333 = B_SPLINE_CURVE_WITH_KNOTS ( 'NONE', 3,
 ( #5660, #1749, #7071, #1099, #456, #1257 ),
 .UNSPECIFIED., .F., .F.,
 ( 4, 2, 4 ),
 ( 2.380731629664482303E-07, 0.002336973833157514335, 0.004673709593152062039 ),
 .UNSPECIFIED. ) ;
#1334 = CARTESIAN_POINT ( 'NONE',  ( 0.000000000000000000, 0.000000000000000000, 16.99999999999991829 ) ) ;
#1335 = ORIENTED_EDGE ( 'NONE', *, *, #5812, .F. ) ;
#1336 = FACE_BOUND ( 'NONE', #5358, .T. ) ;
#1337 = VERTEX_POINT ( 'NONE', #8226 ) ;
#1338 = CARTESIAN_POINT ( 'NONE',  ( 8.000000000000007105, 2.775557561562891351E-14, 6.661338147750939243E-13 ) ) ;
#1339 = UNCERTAINTY_MEASURE_WITH_UNIT (LENGTH_MEASURE( 1.000000000000000082E-05 ), #2325, 'distance_accuracy_value', 'NONE');
#1340 = DIRECTION ( 'NONE',  ( -0.000000000000000000, -1.000000000000000000, -0.000000000000000000 ) ) ;
#1341 = PLANE ( 'NONE',  #7859 ) ;
#1342 = EDGE_CURVE ( 'NONE', #450, #2950, #6967, .T. ) ;
#1343 = CARTESIAN_POINT ( 'NONE',  ( -1.310872448938078083, 8.480771745766464420, -8.082649155111319317 ) ) ;
#1344 = AXIS2_PLACEMENT_3D ( 'NONE', #2202, #2124, #4896 ) ;
#1345 = EDGE_CURVE ( 'NONE', #6377, #4401, #7869, .T. ) ;
#1346 = FACE_OUTER_BOUND ( 'NONE', #4606, .T. ) ;
#1347 = ORIENTED_EDGE ( 'NONE', *, *, #4480, .F. ) ;
#1348 = DIRECTION ( 'NONE',  ( 1.000000000000000000, 8.881784197001244435E-16, 0.000000000000000000 ) ) ;
#1349 = ORIENTED_EDGE ( 'NONE', *, *, #8404, .T. ) ;
#1350 = CARTESIAN_POINT ( 'NONE',  ( -3.318518101603071369, -7.321656987762848345, -8.400000000000021672 ) ) ;
#1351 = ORIENTED_EDGE ( 'NONE', *, *, #4273, .T. ) ;
#1352 = CARTESIAN_POINT ( 'NONE',  ( 20.00000000000011369, -14.99999999999990230, 79.99999999999995737 ) ) ;
#1353 = CARTESIAN_POINT ( 'NONE',  ( -50.00000000000004263, -425.0000000000000000, 25.00000000000001066 ) ) ;
#1354 = CARTESIAN_POINT ( 'NONE',  ( -54.49999999999943867, 152.5000000000003126, 9.999999999999786837 ) ) ;
#1355 = CARTESIAN_POINT ( 'NONE',  ( 3.319543390096077129, -7.321065037175521262, -0.01688885742782669439 ) ) ;
#1356 = LINE ( 'NONE', #7193, #8234 ) ;
#1357 = ORIENTED_EDGE ( 'NONE', *, *, #7546, .F. ) ;
#1358 = DIRECTION ( 'NONE',  ( -1.000000000000000000, -8.881784197001244435E-16, 0.000000000000000000 ) ) ;
#1359 = ORIENTED_EDGE ( 'NONE', *, *, #3242, .T. ) ;
#1360 = SHAPE_DEFINITION_REPRESENTATION ( #8544, #5506 ) ;
#1361 = ADVANCED_BREP_SHAPE_REPRESENTATION ( '', ( #56, #7563 ), #3397 ) ;
#1362 = ADVANCED_FACE ( 'NONE', ( #4951 ), #823, .T. ) ;
#1363 = CARTESIAN_POINT ( 'NONE',  ( 0.000000000000000000, -9.237604307034018802, -0.7145311798163467287 ) ) ;
#1364 = CARTESIAN_POINT ( 'NONE',  ( 5.000000000000115463, -14.99999999999990230, 79.99999999999995737 ) ) ;
#1365 = ORIENTED_EDGE ( 'NONE', *, *, #7801, .T. ) ;
#1366 = CARTESIAN_POINT ( 'NONE',  ( 3.000384657910866768E-15, -410.0000000000000568, -24.50000000000005684 ) ) ;
#1367 = ORIENTED_EDGE ( 'NONE', *, *, #3136, .T. ) ;
#1368 = DIRECTION ( 'NONE',  ( 0.000000000000000000, 0.000000000000000000, -1.000000000000000000 ) ) ;
#1369 = ORIENTED_EDGE ( 'NONE', *, *, #4136, .F. ) ;
#1370 = CARTESIAN_POINT ( 'NONE',  ( -49.99999999999968026, 87.50000000000035527, -1.942890293094023946E-13 ) ) ;
#1371 = ADVANCED_FACE ( 'NONE', ( #1596 ), #244, .F. ) ;
#1372 = DIRECTION ( 'NONE',  ( 1.000000000000000000, 0.000000000000000000, -0.000000000000000000 ) ) ;
#1373 = LINE ( 'NONE', #3940, #7807 ) ;
#1374 = DIRECTION ( 'NONE',  ( 6.400024471206996205E-36, -1.000000000000000000, 0.000000000000000000 ) ) ;
#1375 = DIRECTION ( 'NONE',  ( 3.549874073494553825E-30, -1.000000000000000000, 1.478898702612476446E-15 ) ) ;
#1376 = ORIENTED_EDGE ( 'NONE', *, *, #1782, .T. ) ;
#1377 = CARTESIAN_POINT ( 'NONE',  ( 7.347286611337072948, 4.995646404165303700, -0.4969600502618077842 ) ) ;
#1378 = ORIENTED_EDGE ( 'NONE', *, *, #8008, .F. ) ;
#1379 = FACE_OUTER_BOUND ( 'NONE', #3507, .T. ) ;
#1380 = CONICAL_SURFACE ( 'NONE', #2905, 8.000000000000007105, 1.047197551196597631 ) ;
#1381 = EDGE_CURVE ( 'NONE', #8461, #6830, #3663, .T. ) ;
#1382 = DIRECTION ( 'NONE',  ( 0.000000000000000000, 0.000000000000000000, 1.000000000000000000 ) ) ;
#1383 = CARTESIAN_POINT ( 'NONE',  ( -5.690023276062465385, -5.952467836904175691, -8.269346954796169769 ) ) ;
#1384 = VECTOR ( 'NONE', #3647, 1000.000000000000000 ) ;
#1385 = CARTESIAN_POINT ( 'NONE',  ( 7.999999999999340972, -4.618802153516732290, -7.685468820183672278 ) ) ;
#1386 = LINE ( 'NONE', #4044, #8427 ) ;
#1387 = AXIS2_PLACEMENT_3D ( 'NONE', #1493, #6131, #138 ) ;
#1388 = LINE ( 'NONE', #5356, #4852 ) ;
#1389 = CONICAL_SURFACE ( 'NONE', #3050, 8.000000000000007105, 1.047197551196597631 ) ;
#1390 = CARTESIAN_POINT ( 'NONE',  ( 15.50000000000011191, -14.99999999999990230, -20.00100000000004741 ) ) ;
#1391 = VERTEX_POINT ( 'NONE', #7613 ) ;
#1392 =( GEOMETRIC_REPRESENTATION_CONTEXT ( 3 ) GLOBAL_UNCERTAINTY_ASSIGNED_CONTEXT ( ( #7343 ) ) GLOBAL_UNIT_ASSIGNED_CONTEXT ( ( #774, #7439, #8135 ) ) REPRESENTATION_CONTEXT ( 'NONE', 'WORKASPACE' ) );
#1393 = DIRECTION ( 'NONE',  ( -1.000000000000000000, 2.842664852890546338E-35, 1.540743955509788340E-33 ) ) ;
#1394 = ORIENTED_EDGE ( 'NONE', *, *, #8411, .T. ) ;
#1395 = AXIS2_PLACEMENT_3D ( 'NONE', #5615, #4855, #2986 ) ;
#1396 = ADVANCED_FACE ( 'NONE', ( #6880 ), #7177, .T. ) ;
#1397 = CARTESIAN_POINT ( 'NONE',  ( 5.000000000000115463, -14.99999999999990230, -20.00100000000004741 ) ) ;
#1398 = ORIENTED_EDGE ( 'NONE', *, *, #4013, .T. ) ;
#1399 = DIRECTION ( 'NONE',  ( -1.000000000000000000, 1.774937036747276562E-30, 0.000000000000000000 ) ) ;
#1400 = AXIS2_PLACEMENT_3D ( 'NONE', #2758, #136, #2163 ) ;
#1401 = CONICAL_SURFACE ( 'NONE', #4987, 8.000000000000007105, 1.047197551196597631 ) ;
#1402 = CARTESIAN_POINT ( 'NONE',  ( 33.00000000000055422, -1.390617181863080626E-14, -3.309499999993116504 ) ) ;
#1403 = CARTESIAN_POINT ( 'NONE',  ( 0.000000000000000000, 0.000000000000000000, -109.9999999999999574 ) ) ;
#1404 = VECTOR ( 'NONE', #4018, 1000.000000000000000 ) ;
#1405 = DIRECTION ( 'NONE',  ( -3.328006943901143554E-30, 0.8660254037844380415, -0.5000000000000009992 ) ) ;
#1406 = ORIENTED_EDGE ( 'NONE', *, *, #7155, .T. ) ;
#1407 = AXIS2_PLACEMENT_3D ( 'NONE', #4355, #1009, #878 ) ;
#1408 = ORIENTED_EDGE ( 'NONE', *, *, #5686, .T. ) ;
#1409 = PRESENTATION_LAYER_ASSIGNMENT (  '', '', ( #3897 ) ) ;
#1410 = ADVANCED_FACE ( 'NONE', ( #1631 ), #6923, .F. ) ;
#1411 = PRODUCT_DEFINITION_SHAPE ( 'NONE', 'NONE',  #8607 ) ;
#1412 = DIRECTION ( 'NONE',  ( -1.463706757734299248E-32, 1.000000000000000000, 5.238529448733281520E-32 ) ) ;
#1413 = EDGE_LOOP ( 'NONE', ( #7381, #1188, #6826 ) ) ;
#1414 = CARTESIAN_POINT ( 'NONE',  ( 4.000000000000003553, 6.928203230275597591, 0.000000000000000000 ) ) ;
#1415 = EDGE_CURVE ( 'NONE', #113, #6113, #8014, .T. ) ;
#1416 = ORIENTED_EDGE ( 'NONE', *, *, #2113, .F. ) ;
#1417 = CARTESIAN_POINT ( 'NONE',  ( -8.000000000000000000, -3.867591403079189583, -0.4976753153245850880 ) ) ;
#1418 = ORIENTED_EDGE ( 'NONE', *, *, #3586, .F. ) ;
#1419 = CARTESIAN_POINT ( 'NONE',  ( -6.661338147750939243E-13, -9.237604307034352757, -7.685468820183672278 ) ) ;
#1420 = DIRECTION ( 'NONE',  ( -1.463706757734299248E-32, 1.000000000000000000, 5.238529448733281520E-32 ) ) ;
#1421 = ORIENTED_EDGE ( 'NONE', *, *, #4196, .F. ) ;
#1422 = LINE ( 'NONE', #2550, #7952 ) ;
#1423 =( GEOMETRIC_REPRESENTATION_CONTEXT ( 3 ) GLOBAL_UNCERTAINTY_ASSIGNED_CONTEXT ( ( #7750 ) ) GLOBAL_UNIT_ASSIGNED_CONTEXT ( ( #7929, #7280, #4868 ) ) REPRESENTATION_CONTEXT ( 'NONE', 'WORKASPACE' ) );
#1424 = CARTESIAN_POINT ( 'NONE',  ( 0.000000000000000000, 0.000000000000000000, 0.000000000000000000 ) ) ;
#1425 = EDGE_CURVE ( 'NONE', #6623, #6876, #4129, .T. ) ;
#1426 = LINE ( 'NONE', #2771, #1193 ) ;
#1427 = AXIS2_PLACEMENT_3D ( 'NONE', #5540, #6844, #1518 ) ;
#1428 = LINE ( 'NONE', #6063, #1853 ) ;
#1429 = EDGE_LOOP ( 'NONE', ( #4529, #7281, #7580, #1167 ) ) ;
#1430 = CARTESIAN_POINT ( 'NONE',  ( 5.355005115540953931, 6.145890662064713794, -0.08224679563976165786 ) ) ;
#1431 = SURFACE_STYLE_FILL_AREA ( #8602 ) ;
#1432 = LINE ( 'NONE', #6755, #217 ) ;
#1433 = CARTESIAN_POINT ( 'NONE',  ( 0.000000000000000000, 0.000000000000000000, 0.000000000000000000 ) ) ;
#1434 = EDGE_CURVE ( 'NONE', #3827, #3933, #5578, .T. ) ;
#1435 = CARTESIAN_POINT ( 'NONE',  ( -49.99999999999963762, 87.50000000000035527, 9.999999999999786837 ) ) ;
#1436 = ORIENTED_EDGE ( 'NONE', *, *, #5113, .F. ) ;
#1437 = CARTESIAN_POINT ( 'NONE',  ( 0.000000000000000000, 0.000000000000000000, 0.000000000000000000 ) ) ;
#1438 = VERTEX_POINT ( 'NONE', #6151 ) ;
#1439 = AXIS2_PLACEMENT_3D ( 'NONE', #7332, #1368, #7944 ) ;
#1440 = CARTESIAN_POINT ( 'NONE',  ( 0.000000000000000000, 415.0000000000000000, -19.50000000000002487 ) ) ;
#1441 = DIRECTION ( 'NONE',  ( -1.463706757734299248E-32, 1.000000000000000000, 5.238529448733281520E-32 ) ) ;
#1442 = DIRECTION ( 'NONE',  ( -0.000000000000000000, -0.000000000000000000, 1.000000000000000000 ) ) ;
#1443 = VECTOR ( 'NONE', #3114, 999.9999999999998863 ) ;
#1444 = CARTESIAN_POINT ( 'NONE',  ( 2.309976723937650078, -7.903938623646967088, -0.1306530452038709711 ) ) ;
#1445 = ORIENTED_EDGE ( 'NONE', *, *, #8307, .F. ) ;
#1446 = ADVANCED_FACE ( 'NONE', ( #338 ), #3433, .T. ) ;
#1447 = ORIENTED_EDGE ( 'NONE', *, *, #7891, .T. ) ;
#1448 = AXIS2_PLACEMENT_3D ( 'NONE', #5599, #1778, #4966 ) ;
#1449 = CARTESIAN_POINT ( 'NONE',  ( 9.999999999999896971, 0.000000000000000000, 0.000000000000000000 ) ) ;
#1450 = DIRECTION ( 'NONE',  ( 0.000000000000000000, 0.000000000000000000, -1.000000000000000000 ) ) ;
#1451 = ORIENTED_EDGE ( 'NONE', *, *, #3541, .F. ) ;
#1452 = FACE_OUTER_BOUND ( 'NONE', #7790, .T. ) ;
#1453 = PLANE ( 'NONE',  #7991 ) ;
#1454 = CARTESIAN_POINT ( 'NONE',  ( 461.7368815054782090, 44.30434995311363622, 81.99999999999995737 ) ) ;
#1455 = ORIENTED_EDGE ( 'NONE', *, *, #6569, .T. ) ;
#1456 = DIRECTION ( 'NONE',  ( -1.000000000000000000, -3.083952846180997183E-15, 0.000000000000000000 ) ) ;
#1457 = AXIS2_PLACEMENT_3D ( 'NONE', #3998, #158, #5980 ) ;
#1458 = DIRECTION ( 'NONE',  ( -1.000000000000000000, -8.881784197001244435E-16, 0.000000000000000000 ) ) ;
#1459 = ORIENTED_EDGE ( 'NONE', *, *, #1505, .F. ) ;
#1460 = CARTESIAN_POINT ( 'NONE',  ( 2.220446049250313081E-13, 9.237604307034075646, -8.400000000000018119 ) ) ;
#1461 = EDGE_CURVE ( 'NONE', #7908, #6954, #5531, .T. ) ;
#1462 = CARTESIAN_POINT ( 'NONE',  ( 0.000000000000000000, 0.000000000000000000, -8.400000000000018119 ) ) ;
#1463 = EDGE_LOOP ( 'NONE', ( #4568, #2280, #224 ) ) ;
#1464 = DIRECTION ( 'NONE',  ( 0.000000000000000000, -5.322451846059955323E-30, 1.000000000000000000 ) ) ;
#1465 = DIRECTION ( 'NONE',  ( -1.000000000000000000, 2.842664852890546338E-35, -7.703719777548943412E-34 ) ) ;
#1466 = LINE ( 'NONE', #1940, #6330 ) ;
#1467 = VERTEX_POINT ( 'NONE', #7446 ) ;
#1468 = APPLICATION_CONTEXT ( 'automotive_design' ) ;
#1469 = CARTESIAN_POINT ( 'NONE',  ( 0.000000000000000000, 0.000000000000000000, -8.400000000000018119 ) ) ;
#1470 = CARTESIAN_POINT ( 'NONE',  ( -5.355005115540762084, -6.145890662065133903, -0.08224679563987397080 ) ) ;
#1471 = CONICAL_SURFACE ( 'NONE', #6621, 70.00000000000008527, 0.7853981633974441712 ) ;
#1472 = CARTESIAN_POINT ( 'NONE',  ( -5.355005115540942384, -6.145890662064630305, -0.08224679563972098206 ) ) ;
#1473 = DIRECTION ( 'NONE',  ( -1.000000000000000000, -8.881784197001244435E-16, 0.000000000000000000 ) ) ;
#1474 = DIRECTION ( 'NONE',  ( 1.000000000000000000, 0.000000000000000000, -0.000000000000000000 ) ) ;
#1475 = CYLINDRICAL_SURFACE ( 'NONE', #3816, 5.749999999999984013 ) ;
#1476 = ORIENTED_EDGE ( 'NONE', *, *, #1148, .F. ) ;
#1477 = CARTESIAN_POINT ( 'NONE',  ( -8.000000000000229150, -4.618802153516843312, -0.7145311798163467287 ) ) ;
#1478 = ORIENTED_EDGE ( 'NONE', *, *, #1070, .F. ) ;
#1479 = CARTESIAN_POINT ( 'NONE',  ( -1.313474075707539823, -8.479269695851096245, -0.3167204509600090589 ) ) ;
#1480 = EDGE_CURVE ( 'NONE', #1856, #6375, #5530, .T. ) ;
#1481 = CARTESIAN_POINT ( 'NONE',  ( 8.000000000000229150, -4.440892098500626162E-13, 0.000000000000000000 ) ) ;
#1482 = AXIS2_PLACEMENT_3D ( 'NONE', #2591, #7996, #3985 ) ;
#1483 = ORIENTED_EDGE ( 'NONE', *, *, #6085, .F. ) ;
#1484 = CARTESIAN_POINT ( 'NONE',  ( -49.99999999999944578, 152.5000000000003126, 9.999999999999786837 ) ) ;
#1485 = ORIENTED_EDGE ( 'NONE', *, *, #5280, .F. ) ;
#1486 = MECHANICAL_DESIGN_GEOMETRIC_PRESENTATION_REPRESENTATION (  '', ( #4405 ), #7100 ) ;
#1487 = ORIENTED_EDGE ( 'NONE', *, *, #1489, .F. ) ;
#1488 = AXIS2_PLACEMENT_3D ( 'NONE', #3281, #1937, #5297 ) ;
#1489 = EDGE_CURVE ( 'NONE', #1438, #4229, #7320, .T. ) ;
#1490 = CYLINDRICAL_SURFACE ( 'NONE', #5481, 24.49999999999999645 ) ;
#1491 = EDGE_LOOP ( 'NONE', ( #7153, #7215, #3256 ) ) ;
#1492 = CARTESIAN_POINT ( 'NONE',  ( 1.285879139104719647E-15, 10.49999999999998934, 128.9999999999999432 ) ) ;
#1493 = CARTESIAN_POINT ( 'NONE',  ( 8.000000000000007105, 2.775557561562891351E-14, 6.661338147750939243E-13 ) ) ;
#1494 = DIRECTION ( 'NONE',  ( 0.000000000000000000, 0.000000000000000000, 1.000000000000000000 ) ) ;
#1495 = ORIENTED_EDGE ( 'NONE', *, *, #1461, .T. ) ;
#1496 = VERTEX_POINT ( 'NONE', #3849 ) ;
#1497 = LINE ( 'NONE', #4154, #1568 ) ;
#1498 = EDGE_CURVE ( 'NONE', #2701, #1642, #3574, .T. ) ;
#1499 = DIRECTION ( 'NONE',  ( -0.5000000000000033307, -0.8660254037844367092, 0.000000000000000000 ) ) ;
#1500 = ORIENTED_EDGE ( 'NONE', *, *, #2789, .T. ) ;
#1501 = DIRECTION ( 'NONE',  ( -3.851859888774471706E-33, 7.598173571352219255E-18, -1.000000000000000000 ) ) ;
#1502 = CARTESIAN_POINT ( 'NONE',  ( 0.000000000000000000, -9.237604307034075646, -7.685468820183672278 ) ) ;
#1503 =( NAMED_UNIT ( * ) SI_UNIT ( $, .STERADIAN. ) SOLID_ANGLE_UNIT ( ) );
#1504 = VERTEX_POINT ( 'NONE', #428 ) ;
#1505 = EDGE_CURVE ( 'NONE', #6208, #8158, #1065, .T. ) ;
#1506 = DIRECTION ( 'NONE',  ( 0.000000000000000000, 0.000000000000000000, 1.000000000000000000 ) ) ;
#1507 = B_SPLINE_CURVE_WITH_KNOTS ( 'NONE', 3,
 ( #7211, #6100, #722, #4733, #4031, #3377 ),
 .UNSPECIFIED., .F., .F.,
 ( 4, 2, 4 ),
 ( 0.01291313371729436651, 0.01525081363757299462, 0.01758849355785162272 ),
 .UNSPECIFIED. ) ;
#1508 = CARTESIAN_POINT ( 'NONE',  ( 3.660532965669080152, -7.124194613927820718, -1.655712242656924192E-13 ) ) ;
#1509 = CARTESIAN_POINT ( 'NONE',  ( 5.000000000000004441, -4.685197434473812095, 0.000000000000000000 ) ) ;
#1510 = CARTESIAN_POINT ( 'NONE',  ( -50.00000000000004263, -425.0000000000000000, 25.00000000000001066 ) ) ;
#1511 = CARTESIAN_POINT ( 'NONE',  ( 5.000000000000004441, 0.000000000000000000, 0.000000000000000000 ) ) ;
#1512 = AXIS2_PLACEMENT_3D ( 'NONE', #66, #692, #1474 ) ;
#1513 = DIRECTION ( 'NONE',  ( 1.000000000000000000, 8.881784197001244435E-16, 0.000000000000000000 ) ) ;
#1514 = VERTEX_POINT ( 'NONE', #6507 ) ;
#1515 = VECTOR ( 'NONE', #2255, 1000.000000000000000 ) ;
#1516 = CARTESIAN_POINT ( 'NONE',  ( -7.999999999999888978, -3.867591403079263301, -0.4976753153245478956 ) ) ;
#1517 = ORIENTED_EDGE ( 'NONE', *, *, #7484, .T. ) ;
#1518 = DIRECTION ( 'NONE',  ( 1.000000000000000000, 0.000000000000000000, 0.000000000000000000 ) ) ;
#1519 = CIRCLE ( 'NONE', #6958, 8.000000000000007105 ) ;
#1520 = CARTESIAN_POINT ( 'NONE',  ( 50.00000000000004263, 425.0000000000000000, 25.00000000000000355 ) ) ;
#1521 = ORIENTED_EDGE ( 'NONE', *, *, #6568, .T. ) ;
#1522 = DIRECTION ( 'NONE',  ( 0.000000000000000000, 0.000000000000000000, 1.000000000000000000 ) ) ;
#1523 = ORIENTED_EDGE ( 'NONE', *, *, #2717, .F. ) ;
#1524 = VERTEX_POINT ( 'NONE', #3199 ) ;
#1525 = B_SPLINE_CURVE_WITH_KNOTS ( 'NONE', 3,
 ( #3559, #4032, #6228, #6101, #723, #2205 ),
 .UNSPECIFIED., .F., .F.,
 ( 4, 2, 4 ),
 ( 0.01291313371729497020, 0.01525081363757335544, 0.01758849355785174068 ),
 .UNSPECIFIED. ) ;
#1526 = EDGE_CURVE ( 'NONE', #6748, #2467, #4507, .T. ) ;
#1527 = AXIS2_PLACEMENT_3D ( 'NONE', #8120, #6818, #2275 ) ;
#1528 = FACE_OUTER_BOUND ( 'NONE', #347, .T. ) ;
#1529 = CIRCLE ( 'NONE', #134, 9.499999999999998224 ) ;
#1530 = ORIENTED_EDGE ( 'NONE', *, *, #1704, .F. ) ;
#1531 = CARTESIAN_POINT ( 'NONE',  ( -1.310872448937907997, 8.480771745766357839, -8.082649155111395700 ) ) ;
#1532 = ADVANCED_FACE ( 'NONE', ( #4988 ), #543, .T. ) ;
#1533 = CARTESIAN_POINT ( 'NONE',  ( 0.000000000000000000, 0.000000000000000000, -8.400000000000018119 ) ) ;
#1534 = DIRECTION ( 'NONE',  ( 0.000000000000000000, 0.000000000000000000, -1.000000000000000000 ) ) ;
#1535 = ORIENTED_EDGE ( 'NONE', *, *, #306, .T. ) ;
#1536 = DIRECTION ( 'NONE',  ( -1.000000000000000000, 1.774937036747276562E-30, -0.000000000000000000 ) ) ;
#1537 = ORIENTED_EDGE ( 'NONE', *, *, #4179, .T. ) ;
#1538 = FACE_OUTER_BOUND ( 'NONE', #2078, .T. ) ;
#1539 = MECHANICAL_DESIGN_GEOMETRIC_PRESENTATION_REPRESENTATION (  '', ( #5449 ), #853 ) ;
#1540 = DIRECTION ( 'NONE',  ( 0.000000000000000000, 0.000000000000000000, 1.000000000000000000 ) ) ;
#1541 = CONICAL_SURFACE ( 'NONE', #3775, 8.000000000000007105, 1.047197551196597631 ) ;
#1542 = DIRECTION ( 'NONE',  ( 1.000000000000000000, 0.000000000000000000, 0.000000000000000000 ) ) ;
#1543 = EDGE_LOOP ( 'NONE', ( #4292, #90, #7103, #321, #2523 ) ) ;
#1544 = FACE_OUTER_BOUND ( 'NONE', #1804, .T. ) ;
#1545 = ADVANCED_FACE ( 'NONE', ( #2332 ), #374, .T. ) ;
#1546 =( LENGTH_UNIT ( ) NAMED_UNIT ( * ) SI_UNIT ( .MILLI., .METRE. ) );
#1547 = ORIENTED_EDGE ( 'NONE', *, *, #5549, .T. ) ;
#1548 = ORIENTED_EDGE ( 'NONE', *, *, #5643, .F. ) ;
#1549 = ORIENTED_EDGE ( 'NONE', *, *, #4424, .T. ) ;
#1550 = CARTESIAN_POINT ( 'NONE',  ( -85.74999999999980105, 15.00000000000010836, 10.00000000000017586 ) ) ;
#1551 = DIRECTION ( 'NONE',  ( -1.000000000000000000, 3.549874073494553124E-30, 0.000000000000000000 ) ) ;
#1552 = CARTESIAN_POINT ( 'NONE',  ( 0.000000000000000000, 0.000000000000000000, 0.000000000000000000 ) ) ;
#1553 = CYLINDRICAL_SURFACE ( 'NONE', #8324, 24.50000000000000000 ) ;
#1554 = DIRECTION ( 'NONE',  ( 9.447016907875728896E-60, 5.322451846059955323E-30, -1.000000000000000000 ) ) ;
#1555 = ORIENTED_EDGE ( 'NONE', *, *, #5156, .T. ) ;
#1556 = DIRECTION ( 'NONE',  ( 1.000000000000000000, 0.000000000000000000, 0.000000000000000000 ) ) ;
#1557 = ORIENTED_EDGE ( 'NONE', *, *, #5889, .T. ) ;
#1558 = ADVANCED_FACE ( 'NONE', ( #7044 ), #3696, .F. ) ;
#1559 = CONICAL_SURFACE ( 'NONE', #8242, 8.000000000000007105, 1.047197551196597631 ) ;
#1560 = CARTESIAN_POINT ( 'NONE',  ( -8.000000000000005329, 1.572549600175648044, -0.06894455525513798477 ) ) ;
#1561 = CIRCLE ( 'NONE', #1141, 5.500000000000024869 ) ;
#1562 = EDGE_CURVE ( 'NONE', #947, #2641, #7769, .T. ) ;
#1563 = FACE_OUTER_BOUND ( 'NONE', #2568, .T. ) ;
#1564 = ORIENTED_EDGE ( 'NONE', *, *, #8209, .T. ) ;
#1565 = FACE_OUTER_BOUND ( 'NONE', #5122, .T. ) ;
#1566 = ORIENTED_EDGE ( 'NONE', *, *, #4780, .T. ) ;
#1567 = EDGE_LOOP ( 'NONE', ( #1398, #8035, #25, #870, #250 ) ) ;
#1568 = VECTOR ( 'NONE', #6824, 1000.000000000000000 ) ;
#1569 = LINE ( 'NONE', #2114, #8262 ) ;
#1570 = FILL_AREA_STYLE ('',( #3631 ) ) ;
#1571 = CONICAL_SURFACE ( 'NONE', #180, 8.000000000000007105, 1.047197551196597631 ) ;
#1572 = CARTESIAN_POINT ( 'NONE',  ( -3.319543390096983071, 7.321065037175590540, -0.01688885742807798990 ) ) ;
#1573 = ORIENTED_EDGE ( 'NONE', *, *, #4888, .F. ) ;
#1574 =( GEOMETRIC_REPRESENTATION_CONTEXT ( 3 ) GLOBAL_UNCERTAINTY_ASSIGNED_CONTEXT ( ( #1339 ) ) GLOBAL_UNIT_ASSIGNED_CONTEXT ( ( #2325, #6916, #195 ) ) REPRESENTATION_CONTEXT ( 'NONE', 'WORKASPACE' ) );
#1575 = DIRECTION ( 'NONE',  ( 3.851859888774471706E-33, -7.598173571352223877E-18, 1.000000000000000000 ) ) ;
#1576 = AXIS2_PLACEMENT_3D ( 'NONE', #7579, #7742, #2468 ) ;
#1577 = CARTESIAN_POINT ( 'NONE',  ( -8.000000000000007105, 3.871967595402025175, -7.901061386767586292 ) ) ;
#1578 = DIRECTION ( 'NONE',  ( 4.579669976578770729E-16, 5.898059818321084956E-17, 1.000000000000000000 ) ) ;
#1579 = VERTEX_POINT ( 'NONE', #2421 ) ;
#1580 = CARTESIAN_POINT ( 'NONE',  ( 0.000000000000000000, 0.000000000000000000, 0.000000000000000000 ) ) ;
#1581 = ORIENTED_EDGE ( 'NONE', *, *, #5507, .T. ) ;
#1582 = CARTESIAN_POINT ( 'NONE',  ( 9.999999999999896971, 0.000000000000000000, 79.99999999999995737 ) ) ;
#1583 = AXIS2_PLACEMENT_3D ( 'NONE', #184, #4242, #269 ) ;
#1584 = EDGE_CURVE ( 'NONE', #8094, #2182, #6432, .T. ) ;
#1585 = DIRECTION ( 'NONE',  ( -0.000000000000000000, -0.000000000000000000, 1.000000000000000000 ) ) ;
#1586 = EDGE_LOOP ( 'NONE', ( #187, #442, #4171, #300, #6467, #2482 ) ) ;
#1587 = CARTESIAN_POINT ( 'NONE',  ( 8.000000000000007105, 4.618802153516954334, -8.400000000000018119 ) ) ;
#1588 = EDGE_LOOP ( 'NONE', ( #5037, #2920, #4876, #7419 ) ) ;
#1589 = VERTEX_POINT ( 'NONE', #1076 ) ;
#1590 = ORIENTED_EDGE ( 'NONE', *, *, #2485, .T. ) ;
#1591 = ORIENTED_EDGE ( 'NONE', *, *, #4375, .F. ) ;
#1592 = EDGE_CURVE ( 'NONE', #2559, #2703, #6913, .T. ) ;
#1593 = PRODUCT_DEFINITION_CONTEXT ( 'detailed design', #6520, 'design' ) ;
#1594 = EDGE_CURVE ( 'NONE', #6377, #8133, #7604, .T. ) ;
#1595 = DIRECTION ( 'NONE',  ( 0.000000000000000000, -1.000000000000000000, -1.795949010423047620E-16 ) ) ;
#1596 = FACE_OUTER_BOUND ( 'NONE', #1543, .T. ) ;
#1597 = CARTESIAN_POINT ( 'NONE',  ( 0.000000000000000000, 0.000000000000000000, 0.000000000000000000 ) ) ;
#1598 = CARTESIAN_POINT ( 'NONE',  ( 0.000000000000000000, 0.000000000000000000, -8.400000000000018119 ) ) ;
#1599 = CARTESIAN_POINT ( 'NONE',  ( 0.000000000000000000, 0.000000000000000000, 0.000000000000000000 ) ) ;
#1600 = ORIENTED_EDGE ( 'NONE', *, *, #1062, .F. ) ;
#1601 = CARTESIAN_POINT ( 'NONE',  ( 2.309976723937412491, -7.903938623647039918, -0.1306530452038728585 ) ) ;
#1602 = ORIENTED_EDGE ( 'NONE', *, *, #4265, .F. ) ;
#1603 = EDGE_CURVE ( 'NONE', #3424, #7090, #8161, .T. ) ;
#1604 = DIRECTION ( 'NONE',  ( -1.000000000000000000, 1.774937036747276562E-30, 0.000000000000000000 ) ) ;
#1605 = CARTESIAN_POINT ( 'NONE',  ( -5.354491962338943090, 6.146186931204643322, -8.331901280394173881 ) ) ;
#1606 = EDGE_LOOP ( 'NONE', ( #6094, #8152, #5756 ) ) ;
#1607 = EDGE_LOOP ( 'NONE', ( #1271, #142, #5458, #2317 ) ) ;
#1608 = EDGE_CURVE ( 'NONE', #7519, #2221, #931, .T. ) ;
#1609 = VECTOR ( 'NONE', #4423, 1000.000000000000000 ) ;
#1610 = CARTESIAN_POINT ( 'NONE',  ( 1.313474075707348421, 8.479269695850897293, -8.083279549040144119 ) ) ;
#1611 = CARTESIAN_POINT ( 'NONE',  ( 8.000000000000007105, 4.618802153517065356, -0.7145311798163467287 ) ) ;
#1612 = ORIENTED_EDGE ( 'NONE', *, *, #7834, .T. ) ;
#1613 = DIRECTION ( 'NONE',  ( -1.000000000000000000, 0.000000000000000000, 0.000000000000000000 ) ) ;
#1614 = CIRCLE ( 'NONE', #7737, 5.000000000000034639 ) ;
#1615 = CARTESIAN_POINT ( 'NONE',  ( 1.110223024625156540E-13, -9.237604307034075646, -8.400000000000018119 ) ) ;
#1616 = DIRECTION ( 'NONE',  ( 1.000000000000000000, 0.000000000000000000, 0.000000000000000000 ) ) ;
#1617 = ORIENTED_EDGE ( 'NONE', *, *, #4404, .F. ) ;
#1618 = FACE_OUTER_BOUND ( 'NONE', #7265, .T. ) ;
#1619 = ORIENTED_EDGE ( 'NONE', *, *, #6904, .F. ) ;
#1620 = DIRECTION ( 'NONE',  ( -1.000000000000000000, 2.842664852890546338E-35, 1.540743955509788340E-33 ) ) ;
#1621 = CARTESIAN_POINT ( 'NONE',  ( -7.999999999999896083, -4.618802153517121312, -8.400000000000018119 ) ) ;
#1622 = ORIENTED_EDGE ( 'NONE', *, *, #3019, .T. ) ;
#1623 = CARTESIAN_POINT ( 'NONE',  ( 3.999999999999559464, 6.928203230274987412, 0.000000000000000000 ) ) ;
#1624 = SHAPE_REPRESENTATION_RELATIONSHIP ( 'NONE' , 'NONE' ,  #4603, #2622 ) ;
#1625 = ORIENTED_EDGE ( 'NONE', *, *, #7457, .T. ) ;
#1626 = EDGE_CURVE ( 'NONE', #5659, #5363, #2315, .T. ) ;
#1627 = VERTEX_POINT ( 'NONE', #5759 ) ;
#1628 = CARTESIAN_POINT ( 'NONE',  ( 4.000000000000003553, -1.759474945355333109, 3.047500000000091802 ) ) ;
#1629 = CARTESIAN_POINT ( 'NONE',  ( -19.99999999999986855, 15.00000000000012434, 0.000000000000000000 ) ) ;
#1630 = LINE ( 'NONE', #8267, #7893 ) ;
#1631 = FACE_OUTER_BOUND ( 'NONE', #2344, .T. ) ;
#1632 = CARTESIAN_POINT ( 'NONE',  ( 0.000000000000000000, 0.000000000000000000, 0.000000000000000000 ) ) ;
#1633 = DIRECTION ( 'NONE',  ( 3.919652622816902408E-30, 3.944304526105059027E-30, -1.000000000000000000 ) ) ;
#1634 = EDGE_CURVE ( 'NONE', #2098, #1337, #5074, .T. ) ;
#1635 = DIRECTION ( 'NONE',  ( 0.000000000000000000, 0.000000000000000000, -1.000000000000000000 ) ) ;
#1636 = ORIENTED_EDGE ( 'NONE', *, *, #7048, .T. ) ;
#1637 = ADVANCED_FACE ( 'NONE', ( #1763 ), #3117, .T. ) ;
#1638 = ORIENTED_EDGE ( 'NONE', *, *, #2321, .F. ) ;
#1639 = VECTOR ( 'NONE', #4257, 1000.000000000000000 ) ;
#1640 = AXIS2_PLACEMENT_3D ( 'NONE', #5697, #4444, #310 ) ;
#1641 = CARTESIAN_POINT ( 'NONE',  ( -54.49999999999948841, 152.5000000000003126, -1.942890293094024198E-13 ) ) ;
#1642 = VERTEX_POINT ( 'NONE', #8466 ) ;
#1643 = EDGE_LOOP ( 'NONE', ( #4815, #7980, #4430 ) ) ;
#1644 = EDGE_CURVE ( 'NONE', #8164, #4082, #7498, .T. ) ;
#1645 = FACE_OUTER_BOUND ( 'NONE', #6219, .T. ) ;
#1646 = CARTESIAN_POINT ( 'NONE',  ( 5.000000000000115463, -14.99999999999990230, 0.000000000000000000 ) ) ;
#1647 = EDGE_CURVE ( 'NONE', #758, #8489, #1614, .T. ) ;
#1648 = CARTESIAN_POINT ( 'NONE',  ( -3.660532965669702321, 7.124194613927820718, -3.312531980892385906E-13 ) ) ;
#1649 = DIRECTION ( 'NONE',  ( 0.000000000000000000, 0.000000000000000000, 1.000000000000000000 ) ) ;
#1650 = VERTEX_POINT ( 'NONE', #1 ) ;
#1651 = LINE ( 'NONE', #7798, #7932 ) ;
#1652 = APPLICATION_PROTOCOL_DEFINITION ( 'draft international standard', 'automotive_design', 1998, #5188 ) ;
#1653 = EDGE_LOOP ( 'NONE', ( #738, #8439 ) ) ;
#1654 = CLOSED_SHELL ( 'NONE', ( #6334, #4591, #3818, #7736, #928, #5279, #1681, #7675, #2447, #7657, #2866, #3977, #2237, #8322, #2513, #8157, #6528, #2882, #5191, #5542, #7300, #7524, #7608, #7983, #277, #3644, #5031 ) ) ;
#1655 = CARTESIAN_POINT ( 'NONE',  ( -44.99999999999992895, 425.0000000000000000, 3.122502256758253953E-15 ) ) ;
#1656 = AXIS2_PLACEMENT_3D ( 'NONE', #7038, #8426, #1797 ) ;
#1657 = ADVANCED_FACE ( 'NONE', ( #2684, #5929 ), #5343, .F. ) ;
#1658 = ORIENTED_EDGE ( 'NONE', *, *, #3292, .F. ) ;
#1659 = CYLINDRICAL_SURFACE ( 'NONE', #4214, 50.00000000000008527 ) ;
#1660 = AXIS2_PLACEMENT_3D ( 'NONE', #1364, #4015, #6635 ) ;
#1661 = EDGE_CURVE ( 'NONE', #1337, #4479, #4550, .T. ) ;
#1662 = CARTESIAN_POINT ( 'NONE',  ( 0.000000000000000000, 0.000000000000000000, -8.400000000000018119 ) ) ;
#1663 = VERTEX_POINT ( 'NONE', #6553 ) ;
#1664 = CARTESIAN_POINT ( 'NONE',  ( 38.74999999999992184, 4.806738686653357720E-15, 18.00000000000000355 ) ) ;
#1665 = ORIENTED_EDGE ( 'NONE', *, *, #1608, .T. ) ;
#1666 =( GEOMETRIC_REPRESENTATION_CONTEXT ( 3 ) GLOBAL_UNCERTAINTY_ASSIGNED_CONTEXT ( ( #3671 ) ) GLOBAL_UNIT_ASSIGNED_CONTEXT ( ( #513, #1770, #7866 ) ) REPRESENTATION_CONTEXT ( 'NONE', 'WORKASPACE' ) );
#1667 = EDGE_LOOP ( 'NONE', ( #2472, #3550, #7880, #5878 ) ) ;
#1668 = ORIENTED_EDGE ( 'NONE', *, *, #3869, .T. ) ;
#1669 = DIRECTION ( 'NONE',  ( -3.851859888774471706E-33, 7.598173571352223877E-18, -1.000000000000000000 ) ) ;
#1670 = CYLINDRICAL_SURFACE ( 'NONE', #5189, 80.00000000000000000 ) ;
#1671 = DIRECTION ( 'NONE',  ( 1.463706757734299248E-32, -1.000000000000000000, -5.238529448733281520E-32 ) ) ;
#1672 = ADVANCED_FACE ( 'NONE', ( #765, #2549, #5205 ), #633, .F. ) ;
#1673 = CARTESIAN_POINT ( 'NONE',  ( -50.00000000000004263, -500.0000000000000000, 50.00000000000000000 ) ) ;
#1674 = DIRECTION ( 'NONE',  ( 0.000000000000000000, -1.064348848528640405E-29, 1.000000000000000000 ) ) ;
#1675 = LINE ( 'NONE', #5490, #4722 ) ;
#1676 = CARTESIAN_POINT ( 'NONE',  ( 275.0000000000000000, 425.0000000000000000, 75.00000000000015632 ) ) ;
#1677 = EDGE_LOOP ( 'NONE', ( #1004, #1636 ) ) ;
#1678 = DIRECTION ( 'NONE',  ( -0.000000000000000000, -1.000000000000000000, -0.000000000000000000 ) ) ;
#1679 = EDGE_LOOP ( 'NONE', ( #2046, #5402, #7077, #4475 ) ) ;
#1680 = LINE ( 'NONE', #957, #5485 ) ;
#1681 = ADVANCED_FACE ( 'NONE', ( #7858, #5387 ), #3328, .T. ) ;
#1682 = DIRECTION ( 'NONE',  ( 0.000000000000000000, 0.000000000000000000, -1.000000000000000000 ) ) ;
#1683 = ORIENTED_EDGE ( 'NONE', *, *, #3717, .T. ) ;
#1684 = ORIENTED_EDGE ( 'NONE', *, *, #2466, .F. ) ;
#1685 = CARTESIAN_POINT ( 'NONE',  ( -275.0000000000000000, -425.0000000000000000, 0.000000000000000000 ) ) ;
#1686 = VECTOR ( 'NONE', #7251, 1000.000000000000000 ) ;
#1687 = CIRCLE ( 'NONE', #4903, 39.99999999999999289 ) ;
#1688 = CARTESIAN_POINT ( 'NONE',  ( 3.000384657911015074E-15, -299.9999999999999432, -24.50000000000002842 ) ) ;
#1689 = EDGE_CURVE ( 'NONE', #4831, #4500, #587, .T. ) ;
#1690 = AXIS2_PLACEMENT_3D ( 'NONE', #3227, #5915, #8579 ) ;
#1691 = CARTESIAN_POINT ( 'NONE',  ( -8.000000000000667910, -3.098204225877948303, -8.084209322807835107 ) ) ;
#1692 = CARTESIAN_POINT ( 'NONE',  ( 4.680456609903965948, 6.535341423375566450, -0.01688885742775289925 ) ) ;
#1693 = ORIENTED_EDGE ( 'NONE', *, *, #5772, .T. ) ;
#1694 = AXIS2_PLACEMENT_3D ( 'NONE', #3504, #6179, #5519 ) ;
#1695 = CARTESIAN_POINT ( 'NONE',  ( 0.000000000000000000, 0.000000000000000000, -8.400000000000018119 ) ) ;
#1696 = FACE_OUTER_BOUND ( 'NONE', #1842, .T. ) ;
#1697 = PRODUCT_CONTEXT ( 'NONE', #4636, 'mechanical' ) ;
#1698 = B_SPLINE_CURVE_WITH_KNOTS ( 'NONE', 3,
 ( #3700, #1079, #6364, #3738, #3076, #4466 ),
 .UNSPECIFIED., .F., .F.,
 ( 4, 2, 4 ),
 ( 2.380731626890316258E-07, 0.002336973833157048996, 0.004673709593151410650 ),
 .UNSPECIFIED. ) ;
#1699 = LINE ( 'NONE', #7593, #3623 ) ;
#1700 = CIRCLE ( 'NONE', #5625, 4.499999999999983125 ) ;
#1701 = AXIS2_PLACEMENT_3D ( 'NONE', #5473, #2240, #6910 ) ;
#1702 = CARTESIAN_POINT ( 'NONE',  ( 33.00000000000055422, -1.431146867680865853E-14, 6.883382752675970551E-12 ) ) ;
#1703 = CIRCLE ( 'NONE', #7427, 8.000000000000007105 ) ;
#1704 = EDGE_CURVE ( 'NONE', #5825, #7684, #7052, .T. ) ;
#1705 = DIRECTION ( 'NONE',  ( -6.310887241768093743E-30, 0.8660254037844380415, -0.5000000000000009992 ) ) ;
#1706 = EDGE_LOOP ( 'NONE', ( #2673, #1263, #5085, #5047 ) ) ;
#1707 = AXIS2_PLACEMENT_3D ( 'NONE', #7537, #8149, #7494 ) ;
#1708 = CARTESIAN_POINT ( 'NONE',  ( 8.000000000000007105, 4.618802153516899267, -7.685468820183672278 ) ) ;
#1709 = ORIENTED_EDGE ( 'NONE', *, *, #4035, .T. ) ;
#1710 = CIRCLE ( 'NONE', #585, 8.000000000000007105 ) ;
#1711 = AXIS2_PLACEMENT_3D ( 'NONE', #8438, #7050, #1197 ) ;
#1712 = VERTEX_POINT ( 'NONE', #7296 ) ;
#1713 = ADVANCED_FACE ( 'NONE', ( #8549 ), #6372, .T. ) ;
#1714 = EDGE_CURVE ( 'NONE', #4831, #6936, #797, .T. ) ;
#1715 = CARTESIAN_POINT ( 'NONE',  ( 4.680456609903819398, 6.535341423375429670, -8.383111142572381880 ) ) ;
#1716 = VERTEX_POINT ( 'NONE', #3373 ) ;
#1717 = CARTESIAN_POINT ( 'NONE',  ( -50.00000000000004263, -425.0000000000000000, 3.469446951953614189E-15 ) ) ;
#1718 = CYLINDRICAL_SURFACE ( 'NONE', #1848, 4.250000000000008882 ) ;
#1719 = DIRECTION ( 'NONE',  ( 0.000000000000000000, 0.000000000000000000, 1.000000000000000000 ) ) ;
#1720 =( GEOMETRIC_REPRESENTATION_CONTEXT ( 3 ) GLOBAL_UNCERTAINTY_ASSIGNED_CONTEXT ( ( #1737 ) ) GLOBAL_UNIT_ASSIGNED_CONTEXT ( ( #5710, #8383, #7076 ) ) REPRESENTATION_CONTEXT ( 'NONE', 'WORKASPACE' ) );
#1721 = CARTESIAN_POINT ( 'NONE',  ( 4.000000000000003553, 0.000000000000000000, -3.047500000000091802 ) ) ;
#1722 = CYLINDRICAL_SURFACE ( 'NONE', #3508, 4.250000000000014211 ) ;
#1723 = DIRECTION ( 'NONE',  ( -3.549874073494553124E-30, 1.000000000000000000, -8.626909098572831859E-16 ) ) ;
#1724 = CARTESIAN_POINT ( 'NONE',  ( 8.000000000000007105, -4.618802153517121312, -7.685468820183672278 ) ) ;
#1725 = EDGE_LOOP ( 'NONE', ( #736, #8188 ) ) ;
#1726 = DIRECTION ( 'NONE',  ( 3.451266460341926211E-31, -0.4999999999999985567, 0.8660254037844393737 ) ) ;
#1727 = ORIENTED_EDGE ( 'NONE', *, *, #2733, .T. ) ;
#1728 = CARTESIAN_POINT ( 'NONE',  ( 0.000000000000000000, 9.237604307034130713, -0.7145311798163467287 ) ) ;
#1729 = ITEM_DEFINED_TRANSFORMATION ( 'NONE', 'NONE', #3953,  #7563 ) ;
#1730 = CARTESIAN_POINT ( 'NONE',  ( -6.661338147750939243E-13, 9.237604307034352757, -7.685468820183672278 ) ) ;
#1731 = EDGE_LOOP ( 'NONE', ( #7583, #7141, #2198, #8600, #6128, #1922 ) ) ;
#1732 = ORIENTED_EDGE ( 'NONE', *, *, #3516, .T. ) ;
#1733 = CARTESIAN_POINT ( 'NONE',  ( -32.49999999999997158, 3.469446951953614189E-15, -6.938893903907228378E-15 ) ) ;
#1734 = EDGE_CURVE ( 'NONE', #6936, #2369, #678, .T. ) ;
#1735 =( REPRESENTATION_RELATIONSHIP ('NONE','NONE', #1279, #2536 ) REPRESENTATION_RELATIONSHIP_WITH_TRANSFORMATION ( #3228 )SHAPE_REPRESENTATION_RELATIONSHIP( ) );
#1736 = CIRCLE ( 'NONE', #4957, 8.000000000000007105 ) ;
#1737 = UNCERTAINTY_MEASURE_WITH_UNIT (LENGTH_MEASURE( 1.000000000000000082E-05 ), #5710, 'distance_accuracy_value', 'NONE');
#1738 = PRODUCT_DEFINITION_SHAPE ( 'NONE', 'NONE',  #8626 ) ;
#1739 = CARTESIAN_POINT ( 'NONE',  ( 0.000000000000000000, 0.000000000000000000, -8.401000000000047763 ) ) ;
#1740 = CARTESIAN_POINT ( 'NONE',  ( 0.000000000000000000, 0.000000000000000000, -50.00000000000000000 ) ) ;
#1741 = DIRECTION ( 'NONE',  ( 1.000000000000000000, 8.881784197001244435E-16, 0.000000000000000000 ) ) ;
#1742 = VERTEX_POINT ( 'NONE', #6691 ) ;
#1743 = B_SPLINE_CURVE_WITH_KNOTS ( 'NONE', 3,
 ( #1846, #7165, #3937, #3891, #3197, #5884, #7206, #6550 ),
 .UNSPECIFIED., .F., .F.,
 ( 4, 2, 2, 4 ),
 ( 0.004673709593151984844, 0.005837709341827513297, 0.007001709090503041751, 0.009329708587854099525 ),
 .UNSPECIFIED. ) ;
#1744 = CARTESIAN_POINT ( 'NONE',  ( 5.690023276062453839, 5.952467836904148157, -8.269346954796187532 ) ) ;
#1745 = CARTESIAN_POINT ( 'NONE',  ( -5.500000000000000000, 6.735557395310442023E-16, -50.00000000000000000 ) ) ;
#1746 = DIRECTION ( 'NONE',  ( 1.000000000000000000, 8.736544766236848795E-16, -1.058471975245254351E-16 ) ) ;
#1747 = EDGE_CURVE ( 'NONE', #3875, #4021, #7469, .T. ) ;
#1748 = VECTOR ( 'NONE', #8434, 1000.000000000000000 ) ;
#1749 = CARTESIAN_POINT ( 'NONE',  ( -7.345652830558644375, 4.996589667937334056, -7.903584543331295009 ) ) ;
#1750 = DIRECTION ( 'NONE',  ( 1.000000000000000000, 8.881784197001244435E-16, 0.000000000000000000 ) ) ;
#1751 = ORIENTED_EDGE ( 'NONE', *, *, #2831, .T. ) ;
#1752 = DIRECTION ( 'NONE',  ( 3.919652622816902408E-30, 3.944304526105059027E-30, -1.000000000000000000 ) ) ;
#1753 =( LENGTH_UNIT ( ) NAMED_UNIT ( * ) SI_UNIT ( .MILLI., .METRE. ) );
#1754 = EDGE_LOOP ( 'NONE', ( #8464, #3278, #5220, #7979, #3112 ) ) ;
#1755 = ADVANCED_FACE ( 'NONE', ( #2731 ), #1283, .F. ) ;
#1756 = CARTESIAN_POINT ( 'NONE',  ( 3.000384657911007580E-15, 410.0000000000000000, -24.50000000000004619 ) ) ;
#1757 = ORIENTED_EDGE ( 'NONE', *, *, #1584, .T. ) ;
#1758 = FACE_OUTER_BOUND ( 'NONE', #2934, .T. ) ;
#1759 = EDGE_CURVE ( 'NONE', #4794, #4726, #3149, .T. ) ;
#1760 = VECTOR ( 'NONE', #641, 1000.000000000000000 ) ;
#1761 = DIRECTION ( 'NONE',  ( 1.000000000000000000, -0.000000000000000000, -6.938893903907228378E-17 ) ) ;
#1762 = B_SPLINE_CURVE_WITH_KNOTS ( 'NONE', 3,
 ( #8015, #1516, #831, #7967, #5452, #4706 ),
 .UNSPECIFIED., .F., .F.,
 ( 4, 2, 4 ),
 ( 0.008240550023493596957, 0.01057684187039410230, 0.01291313371729460764 ),
 .UNSPECIFIED. ) ;
#1763 = FACE_OUTER_BOUND ( 'NONE', #4103, .T. ) ;
#1764 = CARTESIAN_POINT ( 'NONE',  ( 1.110223024625156540E-13, 9.237604307033992157, -7.685468820183672278 ) ) ;
#1765 = CARTESIAN_POINT ( 'NONE',  ( 4.000000000000114575, 6.928203230275597591, 0.000000000000000000 ) ) ;
#1766 = ADVANCED_FACE ( 'NONE', ( #6825 ), #2170, .T. ) ;
#1767 = CARTESIAN_POINT ( 'NONE',  ( -6.689127551062020949, -5.375634714784609081, -8.082649155111361949 ) ) ;
#1768 = CYLINDRICAL_SURFACE ( 'NONE', #5918, 39.75000000000007105 ) ;
#1769 = VERTEX_POINT ( 'NONE', #6097 ) ;
#1770 =( NAMED_UNIT ( * ) PLANE_ANGLE_UNIT ( ) SI_UNIT ( $, .RADIAN. ) );
#1771 = EDGE_LOOP ( 'NONE', ( #185, #4295 ) ) ;
#1772 = CIRCLE ( 'NONE', #6248, 8.000000000000007105 ) ;
#1773 = CARTESIAN_POINT ( 'NONE',  ( 2.644994884459373363, -7.710515798486559547, -0.08224679563987125075 ) ) ;
#1774 = CARTESIAN_POINT ( 'NONE',  ( 5.000000000000004441, 0.000000000000000000, 0.000000000000000000 ) ) ;
#1775 = CARTESIAN_POINT ( 'NONE',  ( 5.000000000000115463, -14.99999999999990230, -20.00000000000001776 ) ) ;
#1776 = ORIENTED_EDGE ( 'NONE', *, *, #1381, .F. ) ;
#1777 = FACE_OUTER_BOUND ( 'NONE', #71, .T. ) ;
#1778 = DIRECTION ( 'NONE',  ( 1.000000000000000000, -0.000000000000000000, -6.938893903907228378E-17 ) ) ;
#1779 = CARTESIAN_POINT ( 'NONE',  ( -79.99999999999980105, 15.00000000000012434, 10.00000000000017586 ) ) ;
#1780 = DIRECTION ( 'NONE',  ( -3.851859888774471706E-33, 7.598173571352185358E-18, -1.000000000000000000 ) ) ;
#1781 = FACE_OUTER_BOUND ( 'NONE', #2379, .T. ) ;
#1782 = EDGE_CURVE ( 'NONE', #7684, #7000, #6953, .T. ) ;
#1783 = ORIENTED_EDGE ( 'NONE', *, *, #7377, .T. ) ;
#1784 = DIRECTION ( 'NONE',  ( 1.774937036747276913E-30, -0.5000000000000014433, -0.8660254037844379305 ) ) ;
#1785 = CARTESIAN_POINT ( 'NONE',  ( 50.00000000000004263, -425.0000000000000000, -25.00000000000001066 ) ) ;
#1786 = APPLICATION_CONTEXT ( 'automotive_design' ) ;
#1787 = AXIS2_PLACEMENT_3D ( 'NONE', #4130, #6022, #3257 ) ;
#1788 = CARTESIAN_POINT ( 'NONE',  ( -49.99999999999953815, 120.0000000000003268, 9.999999999999980460 ) ) ;
#1789 = APPLICATION_PROTOCOL_DEFINITION ( 'draft international standard', 'automotive_design', 1998, #5988 ) ;
#1790 = AXIS2_PLACEMENT_3D ( 'NONE', #2424, #3035, #2511 ) ;
#1791 = AXIS2_PLACEMENT_3D ( 'NONE', #3676, #7068, #5743 ) ;
#1792 = VECTOR ( 'NONE', #8077, 1000.000000000000000 ) ;
#1793 = DIRECTION ( 'NONE',  ( -3.549874073494553124E-30, 0.5000000000000009992, 0.8660254037844380415 ) ) ;
#1794 = EDGE_CURVE ( 'NONE', #4055, #4496, #5386, .T. ) ;
#1795 = VERTEX_POINT ( 'NONE', #190 ) ;
#1796 = CLOSED_SHELL ( 'NONE', ( #5165, #5744, #3088, #4851, #318, #262, #4059, #4277, #1170, #4627, #332, #5630, #1766, #4762, #3103 ) ) ;
#1797 = DIRECTION ( 'NONE',  ( 0.000000000000000000, 0.000000000000000000, 1.000000000000000000 ) ) ;
#1798 = CIRCLE ( 'NONE', #271, 39.75000000000007105 ) ;
#1799 = AXIS2_PLACEMENT_3D ( 'NONE', #4331, #2355, #2887 ) ;
#1800 = ORIENTED_EDGE ( 'NONE', *, *, #653, .F. ) ;
#1801 = VECTOR ( 'NONE', #1613, 1000.000000000000000 ) ;
#1802 = MECHANICAL_DESIGN_GEOMETRIC_PRESENTATION_REPRESENTATION (  '', ( #845 ), #2788 ) ;
#1803 = DIRECTION ( 'NONE',  ( 3.919652622816902408E-30, 3.944304526105059027E-30, -1.000000000000000000 ) ) ;
#1804 = EDGE_LOOP ( 'NONE', ( #857, #8356, #4617 ) ) ;
#1805 = CARTESIAN_POINT ( 'NONE',  ( 0.000000000000000000, 3.725716292241969286E-29, -7.000000000000000888 ) ) ;
#1806 = COLOUR_RGB ( '',0.7921568627450980005, 0.8196078431372548767, 0.9333333333333333481 ) ;
#1807 = CARTESIAN_POINT ( 'NONE',  ( -6.661338147750939243E-13, -9.237604307034462892, -8.400000000000018119 ) ) ;
#1808 = EDGE_CURVE ( 'NONE', #5265, #7559, #6096, .T. ) ;
#1809 = PLANE ( 'NONE',  #2954 ) ;
#1810 = CARTESIAN_POINT ( 'NONE',  ( 0.000000000000000000, -9.237604307034018802, -0.7145311798163467287 ) ) ;
#1811 = CIRCLE ( 'NONE', #6412, 4.250000000000010658 ) ;
#1812 = DIRECTION ( 'NONE',  ( 1.000000000000000000, 0.000000000000000000, -6.938893903907228378E-17 ) ) ;
#1813 = CARTESIAN_POINT ( 'NONE',  ( 7.345652830558279334, -4.996589667937374024, -0.4964154566685609615 ) ) ;
#1814 = ORIENTED_EDGE ( 'NONE', *, *, #1268, .F. ) ;
#1815 = FILL_AREA_STYLE_COLOUR ( '', #2510 ) ;
#1816 = ORIENTED_EDGE ( 'NONE', *, *, #8022, .T. ) ;
#1817 = CARTESIAN_POINT ( 'NONE',  ( 0.000000000000000000, 0.000000000000000000, 0.000000000000000000 ) ) ;
#1818 = CONTEXT_DEPENDENT_SHAPE_REPRESENTATION ( #3974, #3417 ) ;
#1819 = LINE ( 'NONE', #5856, #5989 ) ;
#1820 = ORIENTED_EDGE ( 'NONE', *, *, #2733, .F. ) ;
#1821 = CARTESIAN_POINT ( 'NONE',  ( 0.000000000000000000, 0.000000000000000000, -8.400000000000018119 ) ) ;
#1822 = ORIENTED_EDGE ( 'NONE', *, *, #3541, .T. ) ;
#1823 = DIRECTION ( 'NONE',  ( 1.000000000000000000, -2.842664852890546338E-35, -1.540743955509788340E-33 ) ) ;
#1824 = LINE ( 'NONE', #7795, #319 ) ;
#1825 =( NAMED_UNIT ( * ) PLANE_ANGLE_UNIT ( ) SI_UNIT ( $, .RADIAN. ) );
#1826 = EDGE_LOOP ( 'NONE', ( #2329, #3205, #514, #3584 ) ) ;
#1827 = CONICAL_SURFACE ( 'NONE', #7254, 8.000000000000007105, 1.047197551196597631 ) ;
#1828 = CARTESIAN_POINT ( 'NONE',  ( 7.999999999999674039, -4.618802153517231446, -8.400000000000018119 ) ) ;
#1829 = DIRECTION ( 'NONE',  ( 0.000000000000000000, 5.322451846059954622E-30, -1.000000000000000000 ) ) ;
#1830 = DIRECTION ( 'NONE',  ( 0.000000000000000000, 0.000000000000000000, -1.000000000000000000 ) ) ;
#1831 = DIRECTION ( 'NONE',  ( 1.000000000000000000, -5.898059818321126865E-17, -4.579669976578766785E-16 ) ) ;
#1832 = VECTOR ( 'NONE', #7210, 1000.000000000000114 ) ;
#1833 = ADVANCED_FACE ( 'NONE', ( #855 ), #6492, .T. ) ;
#1834 = PRODUCT_RELATED_PRODUCT_CATEGORY ( 'part', '', ( #3271 ) ) ;
#1835 = AXIS2_PLACEMENT_3D ( 'NONE', #1397, #4571, #7970 ) ;
#1836 = CIRCLE ( 'NONE', #2402, 39.75000000000007105 ) ;
#1837 = DIRECTION ( 'NONE',  ( -1.000000000000000000, 0.000000000000000000, 6.938893903907228378E-17 ) ) ;
#1838 = ORIENTED_EDGE ( 'NONE', *, *, #6705, .F. ) ;
#1839 = CARTESIAN_POINT ( 'NONE',  ( 0.000000000000000000, -299.9999999999999432, -2.775557561562891351E-14 ) ) ;
#1840 = CIRCLE ( 'NONE', #23, 8.000000000000007105 ) ;
#1841 = SHAPE_REPRESENTATION_RELATIONSHIP ( 'NONE' , 'NONE' ,  #5506, #5949 ) ;
#1842 = EDGE_LOOP ( 'NONE', ( #2326, #7663, #956, #5195 ) ) ;
#1843 = CIRCLE ( 'NONE', #5629, 0.4000000000000001887 ) ;
#1844 = DIRECTION ( 'NONE',  ( -1.000000000000000000, 3.549874073494553124E-30, 0.000000000000000000 ) ) ;
#1845 = ORIENTED_EDGE ( 'NONE', *, *, #6487, .T. ) ;
#1846 = CARTESIAN_POINT ( 'NONE',  ( 4.000000000000003553, 6.928203230275597591, -8.400000000000018119 ) ) ;
#1847 = EDGE_CURVE ( 'NONE', #922, #4055, #235, .T. ) ;
#1848 = AXIS2_PLACEMENT_3D ( 'NONE', #4387, #5672, #5803 ) ;
#1849 = DIRECTION ( 'NONE',  ( 0.000000000000000000, 0.000000000000000000, 1.000000000000000000 ) ) ;
#1850 = CARTESIAN_POINT ( 'NONE',  ( 32.49999999999997158, 1.387778780781445676E-14, 18.00000000000000355 ) ) ;
#1851 = DIRECTION ( 'NONE',  ( -1.463706757734299248E-32, 1.000000000000000000, 5.238529448733281520E-32 ) ) ;
#1852 = VECTOR ( 'NONE', #6126, 1000.000000000000000 ) ;
#1853 = VECTOR ( 'NONE', #637, 1000.000000000000000 ) ;
#1854 = CARTESIAN_POINT ( 'NONE',  ( -1.310872448937806745, 8.480771745766437775, -8.082649155111361949 ) ) ;
#1855 = VERTEX_POINT ( 'NONE', #810 ) ;
#1856 = VERTEX_POINT ( 'NONE', #4248 ) ;
#1857 = DIRECTION ( 'NONE',  ( -1.000000000000000000, 3.549874073494553124E-30, 0.000000000000000000 ) ) ;
#1858 = VECTOR ( 'NONE', #877, 1000.000000000000000 ) ;
#1859 = B_SPLINE_CURVE_WITH_KNOTS ( 'NONE', 3,
 ( #3081, #6795, #6653, #1430, #61, #2774, #1377, #2032 ),
 .UNSPECIFIED., .F., .F.,
 ( 4, 2, 2, 4 ),
 ( 0.004673709593151983109, 0.005837709341827512430, 0.007001709090503040883, 0.009329708587854099525 ),
 .UNSPECIFIED. ) ;
#1860 = ADVANCED_FACE ( 'NONE', ( #145 ), #3158, .T. ) ;
#1861 = AXIS2_PLACEMENT_3D ( 'NONE', #5515, #8163, #2197 ) ;
#1862 = CARTESIAN_POINT ( 'NONE',  ( -50.00000000000004263, 500.0000000000000000, 50.00000000000000000 ) ) ;
#1863 = LINE ( 'NONE', #603, #7517 ) ;
#1864 = CARTESIAN_POINT ( 'NONE',  ( 8.000000000000007105, 4.618802153517065356, -7.685468820183672278 ) ) ;
#1865 = ITEM_DEFINED_TRANSFORMATION ( 'NONE', 'NONE', #1583,  #7563 ) ;
#1866 = ORIENTED_EDGE ( 'NONE', *, *, #6415, .F. ) ;
#1867 = DIRECTION ( 'NONE',  ( -3.919652622816902408E-30, -3.944304526105059027E-30, 1.000000000000000000 ) ) ;
#1868 = EDGE_LOOP ( 'NONE', ( #443, #5994, #2835, #8154 ) ) ;
#1869 = DIRECTION ( 'NONE',  ( -1.000000000000000000, -8.881784197001244435E-16, 0.000000000000000000 ) ) ;
#1870 = AXIS2_PLACEMENT_3D ( 'NONE', #7070, #1098, #3143 ) ;
#1871 = ORIENTED_EDGE ( 'NONE', *, *, #8153, .T. ) ;
#1872 = EDGE_CURVE ( 'NONE', #988, #1514, #2766, .T. ) ;
#1873 = DIRECTION ( 'NONE',  ( -0.9237280213470678847, -0.3830490080632384942, 0.000000000000000000 ) ) ;
#1874 = CONICAL_SURFACE ( 'NONE', #8141, 8.000000000000007105, 1.047197551196597631 ) ;
#1875 = DIRECTION ( 'NONE',  ( -1.774937036747276562E-30, 1.000000000000000000, -1.110768649713241713E-15 ) ) ;
#1876 = CARTESIAN_POINT ( 'NONE',  ( 0.7999999999999674039, -1.387778780781445676E-14, 0.000000000000000000 ) ) ;
#1877 = CARTESIAN_POINT ( 'NONE',  ( 8.000000000000234479, -0.7805016046292200249, -1.407040310002008213E-13 ) ) ;
#1878 = CYLINDRICAL_SURFACE ( 'NONE', #4599, 25.00000000000000711 ) ;
#1879 = ORIENTED_EDGE ( 'NONE', *, *, #2820, .T. ) ;
#1880 = CARTESIAN_POINT ( 'NONE',  ( 0.000000000000000000, 0.000000000000000000, 10.00000000000000178 ) ) ;
#1881 = AXIS2_PLACEMENT_3D ( 'NONE', #2639, #4555, #7817 ) ;
#1882 = CONTEXT_DEPENDENT_SHAPE_REPRESENTATION ( #1300, #1411 ) ;
#1883 = DIRECTION ( 'NONE',  ( 3.919652622816902408E-30, 3.944304526105059027E-30, -1.000000000000000000 ) ) ;
#1884 = ORIENTED_EDGE ( 'NONE', *, *, #5073, .T. ) ;
#1885 = DIRECTION ( 'NONE',  ( -1.000000000000000000, 1.774937036747276562E-30, 0.000000000000000000 ) ) ;
#1886 = AXIS2_PLACEMENT_3D ( 'NONE', #4613, #5940, #8007 ) ;
#1887 = EDGE_LOOP ( 'NONE', ( #4243, #5608 ) ) ;
#1888 = DIRECTION ( 'NONE',  ( 0.000000000000000000, 0.000000000000000000, 1.000000000000000000 ) ) ;
#1889 = ORIENTED_EDGE ( 'NONE', *, *, #6867, .T. ) ;
#1890 = CARTESIAN_POINT ( 'NONE',  ( 0.000000000000000000, -4.685197434473812983, 0.000000000000000000 ) ) ;
#1891 = CARTESIAN_POINT ( 'NONE',  ( 2.309976723937405829, -7.903938623647046136, -8.269346954796146676 ) ) ;
#1892 = AXIS2_PLACEMENT_3D ( 'NONE', #6921, #776, #2136 ) ;
#1893 = DIRECTION ( 'NONE',  ( -0.000000000000000000, -0.000000000000000000, 1.000000000000000000 ) ) ;
#1894 = CARTESIAN_POINT ( 'NONE',  ( 0.000000000000000000, 0.000000000000000000, 79.99999999999995737 ) ) ;
#1895 = DIRECTION ( 'NONE',  ( 1.000000000000000000, 0.000000000000000000, -6.938893903907228378E-17 ) ) ;
#1896 = ADVANCED_FACE ( 'NONE', ( #7474 ), #3599, .T. ) ;
#1897 = CARTESIAN_POINT ( 'NONE',  ( -7.999999999999785061, -4.618802153517121312, -8.400000000000018119 ) ) ;
#1898 = CARTESIAN_POINT ( 'NONE',  ( -2.309976723937442245, 7.903938623646887152, -8.269346954796224836 ) ) ;
#1899 = ORIENTED_EDGE ( 'NONE', *, *, #2809, .F. ) ;
#1900 = AXIS2_PLACEMENT_3D ( 'NONE', #3813, #1671, #2374 ) ;
#1901 = ORIENTED_EDGE ( 'NONE', *, *, #3069, .T. ) ;
#1902 = DIRECTION ( 'NONE',  ( 0.000000000000000000, 0.000000000000000000, -1.000000000000000000 ) ) ;
#1903 = CIRCLE ( 'NONE', #3449, 5.749999999999985789 ) ;
#1904 = PLANE ( 'NONE',  #3247 ) ;
#1905 = FACE_OUTER_BOUND ( 'NONE', #5900, .T. ) ;
#1906 = CARTESIAN_POINT ( 'NONE',  ( 50.00000000000004263, 425.0000000000000000, -25.00000000000001066 ) ) ;
#1907 = CARTESIAN_POINT ( 'NONE',  ( -38.74999999999992184, -5.658996171085535125E-33, 18.00000000000000355 ) ) ;
#1908 = DIRECTION ( 'NONE',  ( -2.842664852890546338E-35, 1.000000000000000000, -2.189909344815615958E-68 ) ) ;
#1909 = APPLICATION_CONTEXT ( 'automotive_design' ) ;
#1910 = ORIENTED_EDGE ( 'NONE', *, *, #5829, .F. ) ;
#1911 = DIRECTION ( 'NONE',  ( -1.463706757734299248E-32, 1.000000000000000000, 5.238529448733281520E-32 ) ) ;
#1912 = EDGE_CURVE ( 'NONE', #1589, #5078, #1772, .T. ) ;
#1913 = ORIENTED_EDGE ( 'NONE', *, *, #2767, .T. ) ;
#1914 = ORIENTED_EDGE ( 'NONE', *, *, #6448, .F. ) ;
#1915 = CARTESIAN_POINT ( 'NONE',  ( 4.000000000000003553, 9.714451465470119729E-14, 0.000000000000000000 ) ) ;
#1916 = ORIENTED_EDGE ( 'NONE', *, *, #4023, .T. ) ;
#1917 = DIRECTION ( 'NONE',  ( 3.851859888774471706E-33, -7.598173571352223877E-18, 1.000000000000000000 ) ) ;
#1918 = CARTESIAN_POINT ( 'NONE',  ( 9.999999999999896971, 0.000000000000000000, 0.000000000000000000 ) ) ;
#1919 = CARTESIAN_POINT ( 'NONE',  ( 275.0000000000000000, -425.0000000000000000, -80.00000000000000000 ) ) ;
#1920 = DIRECTION ( 'NONE',  ( 3.919652622816902408E-30, 3.944304526105059027E-30, -1.000000000000000000 ) ) ;
#1921 = PRESENTATION_STYLE_ASSIGNMENT (( #5231 ) ) ;
#1922 = ORIENTED_EDGE ( 'NONE', *, *, #5590, .F. ) ;
#1923 = ADVANCED_FACE ( 'NONE', ( #4853 ), #2284, .T. ) ;
#1924 = DIRECTION ( 'NONE',  ( 3.851859888774471706E-33, 1.232595164407830946E-32, 1.000000000000000000 ) ) ;
#1925 = SURFACE_SIDE_STYLE ('',( #5237 ) ) ;
#1926 = EDGE_CURVE ( 'NONE', #92, #3910, #3735, .T. ) ;
#1927 = EDGE_CURVE ( 'NONE', #5903, #2515, #2855, .T. ) ;
#1928 = LINE ( 'NONE', #4589, #114 ) ;
#1929 = EDGE_LOOP ( 'NONE', ( #7074, #35, #5212, #617 ) ) ;
#1930 = AXIS2_PLACEMENT_3D ( 'NONE', #3172, #8488, #2522 ) ;
#1931 = AXIS2_PLACEMENT_3D ( 'NONE', #2061, #6542, #8583 ) ;
#1932 = CARTESIAN_POINT ( 'NONE',  ( 8.000000000000007105, 4.618802153516732290, -8.400000000000018119 ) ) ;
#1933 = ORIENTED_EDGE ( 'NONE', *, *, #7521, .T. ) ;
#1934 = CARTESIAN_POINT ( 'NONE',  ( 1.355854680848614041E-28, -410.0000000000000568, 24.49999999999991829 ) ) ;
#1935 = EDGE_LOOP ( 'NONE', ( #6404, #7360, #7630 ) ) ;
#1936 = EDGE_CURVE ( 'NONE', #2349, #2603, #3753, .T. ) ;
#1937 = DIRECTION ( 'NONE',  ( 3.851859888774471706E-33, 1.232595164407830946E-32, 1.000000000000000000 ) ) ;
#1938 = FACE_OUTER_BOUND ( 'NONE', #1643, .T. ) ;
#1939 = DIRECTION ( 'NONE',  ( -3.851859888774471706E-33, 7.598173571352223877E-18, -1.000000000000000000 ) ) ;
#1940 = CARTESIAN_POINT ( 'NONE',  ( -50.00000000000004263, 425.0000000000000000, 25.00000000000001066 ) ) ;
#1941 = EDGE_LOOP ( 'NONE', ( #8445, #8072, #6080 ) ) ;
#1942 = SHAPE_REPRESENTATION ( 'hex nut style 1_am_B18.2.4.1M - Hex nut, Style 1,  M10 x 1.5, with 16mm WAF --D-N', ( #7563 ), #4502 ) ;
#1943 = CONICAL_SURFACE ( 'NONE', #2642, 3.047499999999999876, 1.047197551196592524 ) ;
#1944 = VECTOR ( 'NONE', #1146, 1000.000000000000000 ) ;
#1945 = CARTESIAN_POINT ( 'NONE',  ( 0.000000000000000000, 32.50000000000005684, -6.938893903907228378E-15 ) ) ;
#1946 = EDGE_LOOP ( 'NONE', ( #100, #2888, #6161, #6293, #390, #5727 ) ) ;
#1947 = FACE_OUTER_BOUND ( 'NONE', #236, .T. ) ;
#1948 = AXIS2_PLACEMENT_3D ( 'NONE', #6351, #1069, #7075 ) ;
#1949 = EDGE_CURVE ( 'NONE', #2390, #3139, #7384, .T. ) ;
#1950 = CARTESIAN_POINT ( 'NONE',  ( 7.999999999999563016, -4.618802153517398423, -0.7145311798163467287 ) ) ;
#1951 = AXIS2_PLACEMENT_3D ( 'NONE', #1437, #6842, #3482 ) ;
#1952 = CARTESIAN_POINT ( 'NONE',  ( -21.99999999999954881, 120.0000000000003126, 9.999999999999980460 ) ) ;
#1953 = ORIENTED_EDGE ( 'NONE', *, *, #875, .F. ) ;
#1954 = FACE_BOUND ( 'NONE', #7294, .T. ) ;
#1955 = AXIS2_PLACEMENT_3D ( 'NONE', #3957, #5976, #8006 ) ;
#1956 = ORIENTED_EDGE ( 'NONE', *, *, #930, .T. ) ;
#1957 = ORIENTED_EDGE ( 'NONE', *, *, #3170, .T. ) ;
#1958 = CARTESIAN_POINT ( 'NONE',  ( 0.000000000000000000, 0.000000000000000000, 5.551115123125782702E-14 ) ) ;
#1959 = ORIENTED_EDGE ( 'NONE', *, *, #6846, .F. ) ;
#1960 = DIRECTION ( 'NONE',  ( -1.000000000000000000, -8.881784197001244435E-16, 0.000000000000000000 ) ) ;
#1961 = AXIS2_PLACEMENT_3D ( 'NONE', #4989, #5805, #8467 ) ;
#1962 = EDGE_CURVE ( 'NONE', #2182, #8418, #8061, .T. ) ;
#1963 = FACE_BOUND ( 'NONE', #8536, .T. ) ;
#1964 = CARTESIAN_POINT ( 'NONE',  ( 0.000000000000000000, 0.000000000000000000, -8.400000000000018119 ) ) ;
#1965 = FILL_AREA_STYLE_COLOUR ( '', #3198 ) ;
#1966 = ORIENTED_EDGE ( 'NONE', *, *, #4642, .T. ) ;
#1967 = DIRECTION ( 'NONE',  ( -1.000000000000000000, 0.000000000000000000, 0.000000000000000000 ) ) ;
#1968 = EDGE_CURVE ( 'NONE', #5323, #2931, #2361, .T. ) ;
#1969 = ADVANCED_BREP_SHAPE_REPRESENTATION ( '', ( #5834, #7563 ), #4502 ) ;
#1970 = EDGE_LOOP ( 'NONE', ( #4625, #583, #3432, #353, #6761, #8091 ) ) ;
#1971 = CARTESIAN_POINT ( 'NONE',  ( 5.000000000000004441, 4.685197434473897360, 0.000000000000000000 ) ) ;
#1972 = SHAPE_REPRESENTATION_RELATIONSHIP ( 'NONE' , 'NONE' ,  #1942, #1969 ) ;
#1973 = ORIENTED_EDGE ( 'NONE', *, *, #7824, .T. ) ;
#1974 = CIRCLE ( 'NONE', #580, 10.00000000000000178 ) ;
#1975 = AXIS2_PLACEMENT_3D ( 'NONE', #562, #72, #5946 ) ;
#1976 = CARTESIAN_POINT ( 'NONE',  ( 0.000000000000000000, -500.0000000000000000, 0.000000000000000000 ) ) ;
#1977 = ORIENTED_EDGE ( 'NONE', *, *, #8268, .F. ) ;
#1978 = CARTESIAN_POINT ( 'NONE',  ( 5.500000000000000000, 0.000000000000000000, -50.00000000000000000 ) ) ;
#1979 = EDGE_CURVE ( 'NONE', #6357, #6260, #416, .T. ) ;
#1980 = AXIS2_PLACEMENT_3D ( 'NONE', #7324, #4010, #6037 ) ;
#1981 = DIRECTION ( 'NONE',  ( 0.000000000000000000, 0.000000000000000000, 1.000000000000000000 ) ) ;
#1982 = CARTESIAN_POINT ( 'NONE',  ( 0.000000000000000000, 0.000000000000000000, -8.400000000000018119 ) ) ;
#1983 = AXIS2_PLACEMENT_3D ( 'NONE', #5865, #3832, #4580 ) ;
#1984 = AXIS2_PLACEMENT_3D ( 'NONE', #1976, #2679, #3369 ) ;
#1985 = LINE ( 'NONE', #3333, #7711 ) ;
#1986 = DIRECTION ( 'NONE',  ( 0.000000000000000000, 0.000000000000000000, -1.000000000000000000 ) ) ;
#1987 = VERTEX_POINT ( 'NONE', #5663 ) ;
#1988 = CARTESIAN_POINT ( 'NONE',  ( 1.110223024625156540E-13, -414.9999999999999432, -4.163336342344337027E-14 ) ) ;
#1989 = VERTEX_POINT ( 'NONE', #6387 ) ;
#1990 = DIRECTION ( 'NONE',  ( -0.8660254037844365982, 0.5000000000000035527, -0.000000000000000000 ) ) ;
#1991 = AXIS2_PLACEMENT_3D ( 'NONE', #3266, #6715, #8574 ) ;
#1992 = CARTESIAN_POINT ( 'NONE',  ( 0.000000000000000000, 500.0000000000000000, 0.000000000000000000 ) ) ;
#1993 = EDGE_CURVE ( 'NONE', #4021, #3875, #4723, .T. ) ;
#1994 = CARTESIAN_POINT ( 'NONE',  ( -275.0000000000000000, -425.0000000000000000, 0.000000000000000000 ) ) ;
#1995 = CARTESIAN_POINT ( 'NONE',  ( -49.99999999999968026, 87.50000000000035527, -1.942890293094023946E-13 ) ) ;
#1996 =( GEOMETRIC_REPRESENTATION_CONTEXT ( 3 ) GLOBAL_UNCERTAINTY_ASSIGNED_CONTEXT ( ( #4363 ) ) GLOBAL_UNIT_ASSIGNED_CONTEXT ( ( #6312, #8302, #991 ) ) REPRESENTATION_CONTEXT ( 'NONE', 'WORKASPACE' ) );
#1997 = CARTESIAN_POINT ( 'NONE',  ( 3.660532965669079708, -7.124194613927820718, -8.399999999999852918 ) ) ;
#1998 = CARTESIAN_POINT ( 'NONE',  ( -7.345652830558973889, 4.996589667937345602, -7.903584543331135137 ) ) ;
#1999 = VERTEX_POINT ( 'NONE', #6348 ) ;
#2000 = FACE_BOUND ( 'NONE', #8112, .T. ) ;
#2001 = ORIENTED_EDGE ( 'NONE', *, *, #5652, .F. ) ;
#2002 = AXIS2_PLACEMENT_3D ( 'NONE', #3465, #6737, #2763 ) ;
#2003 = CARTESIAN_POINT ( 'NONE',  ( -0.6543471694412575923, -8.859816792613658620, -7.903584543331218626 ) ) ;
#2004 = EDGE_LOOP ( 'NONE', ( #670, #6292 ) ) ;
#2005 = DIRECTION ( 'NONE',  ( 0.000000000000000000, 0.000000000000000000, 1.000000000000000000 ) ) ;
#2006 = CARTESIAN_POINT ( 'NONE',  ( 8.000000000000122569, 0.7809653281574673311, -6.100924209188546528E-14 ) ) ;
#2007 = CARTESIAN_POINT ( 'NONE',  ( 4.000000000000003553, 9.714451465470119729E-14, 0.000000000000000000 ) ) ;
#2008 = DIRECTION ( 'NONE',  ( 0.000000000000000000, 0.000000000000000000, 1.000000000000000000 ) ) ;
#2009 = VERTEX_POINT ( 'NONE', #3147 ) ;
#2010 = AXIS2_PLACEMENT_3D ( 'NONE', #5059, #3182, #8455 ) ;
#2011 = VERTEX_POINT ( 'NONE', #413 ) ;
#2012 = ADVANCED_FACE ( 'NONE', ( #5099 ), #268, .T. ) ;
#2013 = PRODUCT_CONTEXT ( 'NONE', #5779, 'mechanical' ) ;
#2014 = ORIENTED_EDGE ( 'NONE', *, *, #4013, .F. ) ;
#2015 = EDGE_CURVE ( 'NONE', #232, #3217, #6423, .T. ) ;
#2016 = FACE_BOUND ( 'NONE', #7479, .T. ) ;
#2017 = ADVANCED_FACE ( 'NONE', ( #5749 ), #3645, .F. ) ;
#2018 = CARTESIAN_POINT ( 'NONE',  ( 0.000000000000000000, 415.0000000000000000, -5.551115123125782702E-14 ) ) ;
#2019 = DIRECTION ( 'NONE',  ( 0.000000000000000000, 0.000000000000000000, 1.000000000000000000 ) ) ;
#2020 = VERTEX_POINT ( 'NONE', #7802 ) ;
#2021 = CARTESIAN_POINT ( 'NONE',  ( 5.690023276062378343, 5.952467836904126841, -8.269346954796224836 ) ) ;
#2022 = ORIENTED_EDGE ( 'NONE', *, *, #1949, .F. ) ;
#2023 = LINE ( 'NONE', #3324, #3942 ) ;
#2024 = VECTOR ( 'NONE', #345, 1000.000000000000000 ) ;
#2025 = DIRECTION ( 'NONE',  ( -0.000000000000000000, -0.000000000000000000, 1.000000000000000000 ) ) ;
#2026 = VECTOR ( 'NONE', #4909, 1000.000000000000000 ) ;
#2027 = LINE ( 'NONE', #1331, #3362 ) ;
#2028 = FACE_OUTER_BOUND ( 'NONE', #207, .T. ) ;
#2029 = ADVANCED_FACE ( 'NONE', ( #1031 ), #6308, .F. ) ;
#2030 = CARTESIAN_POINT ( 'NONE',  ( 5.355005115540955707, 6.145890662064651622, -0.08224679563973515128 ) ) ;
#2031 = ORIENTED_EDGE ( 'NONE', *, *, #3184, .F. ) ;
#2032 = CARTESIAN_POINT ( 'NONE',  ( 8.000000000000117240, 4.618802153517009401, -0.7145311798163467287 ) ) ;
#2033 = FACE_OUTER_BOUND ( 'NONE', #6919, .T. ) ;
#2034 = FACE_OUTER_BOUND ( 'NONE', #3215, .T. ) ;
#2035 = B_SPLINE_CURVE_WITH_KNOTS ( 'NONE', 3,
 ( #7321, #5410, #1355, #4799, #1444, #6672, #4054, #8062 ),
 .UNSPECIFIED., .F., .F.,
 ( 4, 2, 2, 4 ),
 ( 0.004673709593152262400, 0.005837709341827771771, 0.007001709090503281142, 0.009329708587854299018 ),
 .UNSPECIFIED. ) ;
#2036 = CARTESIAN_POINT ( 'NONE',  ( 8.000000000000238032, -3.098204225878338658, -8.084209322807982545 ) ) ;
#2037 = CARTESIAN_POINT ( 'NONE',  ( -5.499999999999999112, 60.00000000000000000, 45.00000000000000000 ) ) ;
#2038 = EDGE_CURVE ( 'NONE', #2131, #3744, #3892, .T. ) ;
#2039 = CARTESIAN_POINT ( 'NONE',  ( 0.000000000000000000, 0.000000000000000000, -8.400000000000018119 ) ) ;
#2040 = CARTESIAN_POINT ( 'NONE',  ( -44.99999999999992895, -425.0000000000000000, -25.00000000000000355 ) ) ;
#2041 = CARTESIAN_POINT ( 'NONE',  ( -3.319543390096230340, 7.321065037175420009, -8.383111142572211349 ) ) ;
#2042 = CARTESIAN_POINT ( 'NONE',  ( -8.000000000000007105, 0.000000000000000000, -8.400000000000018119 ) ) ;
#2043 = ORIENTED_EDGE ( 'NONE', *, *, #5848, .T. ) ;
#2044 = B_SPLINE_CURVE_WITH_KNOTS ( 'NONE', 3,
 ( #1502, #5566, #771, #8216, #3427, #5437 ),
 .UNSPECIFIED., .F., .F.,
 ( 4, 2, 4 ),
 ( 2.380731630569847498E-07, 0.002336973833157701252, 0.004673709593152344799 ),
 .UNSPECIFIED. ) ;
#2045 = LINE ( 'NONE', #784, #5137 ) ;
#2046 = ORIENTED_EDGE ( 'NONE', *, *, #786, .F. ) ;
#2047 = DIRECTION ( 'NONE',  ( 1.000000000000000000, -3.549874073494553124E-30, -3.778304382545602261E-59 ) ) ;
#2048 = ORIENTED_EDGE ( 'NONE', *, *, #5752, .F. ) ;
#2049 = CARTESIAN_POINT ( 'NONE',  ( 50.00000000000004263, 500.0000000000000000, 45.00000000000000711 ) ) ;
#2050 = CARTESIAN_POINT ( 'NONE',  ( -2.560009788482805538E-34, 40.00000000000007816, 3.039269428540890907E-16 ) ) ;
#2051 = EDGE_CURVE ( 'NONE', #2597, #579, #5794, .T. ) ;
#2052 = VECTOR ( 'NONE', #5366, 1000.000000000000000 ) ;
#2053 = CARTESIAN_POINT ( 'NONE',  ( -50.00000000000004263, 500.0000000000000000, 50.00000000000000000 ) ) ;
#2054 = VERTEX_POINT ( 'NONE', #1142 ) ;
#2055 = ORIENTED_EDGE ( 'NONE', *, *, #6812, .F. ) ;
#2056 =( NAMED_UNIT ( * ) PLANE_ANGLE_UNIT ( ) SI_UNIT ( $, .RADIAN. ) );
#2057 = DIRECTION ( 'NONE',  ( 1.000000000000000000, 0.000000000000000000, 0.000000000000000000 ) ) ;
#2058 = EDGE_CURVE ( 'NONE', #3844, #4655, #7635, .T. ) ;
#2059 = DIRECTION ( 'NONE',  ( 0.000000000000000000, 0.000000000000000000, 1.000000000000000000 ) ) ;
#2060 = CIRCLE ( 'NONE', #4573, 4.000000000000030198 ) ;
#2061 = CARTESIAN_POINT ( 'NONE',  ( 0.000000000000000000, 0.000000000000000000, -8.400000000000018119 ) ) ;
#2062 = EDGE_LOOP ( 'NONE', ( #3028, #7325 ) ) ;
#2063 = B_SPLINE_CURVE_WITH_KNOTS ( 'NONE', 3,
 ( #7881, #5504, #4619, #3398, #4002, #7271 ),
 .UNSPECIFIED., .F., .F.,
 ( 4, 2, 4 ),
 ( 0.008240550023493595222, 0.01057684187039410403, 0.01291313371729461111 ),
 .UNSPECIFIED. ) ;
#2064 = CARTESIAN_POINT ( 'NONE',  ( 2.220446049250313081E-13, 9.237604307034075646, -0.7145311798163467287 ) ) ;
#2065 = DIRECTION ( 'NONE',  ( -8.240196998932437191E-18, -0.2702506080694626611, -0.9627900128470828767 ) ) ;
#2066 = EDGE_LOOP ( 'NONE', ( #5222, #5126, #6989, #2981 ) ) ;
#2067 =( REPRESENTATION_RELATIONSHIP ('NONE','NONE', #1279, #4003 ) REPRESENTATION_RELATIONSHIP_WITH_TRANSFORMATION ( #7743 )SHAPE_REPRESENTATION_RELATIONSHIP( ) );
#2068 = CARTESIAN_POINT ( 'NONE',  ( -5.080504117408889186, -2.106769544347818268, -8.400000000000018119 ) ) ;
#2069 = VERTEX_POINT ( 'NONE', #987 ) ;
#2070 = PLANE ( 'NONE',  #4205 ) ;
#2071 = ADVANCED_FACE ( 'NONE', ( #2984 ), #4376, .F. ) ;
#2072 = EDGE_CURVE ( 'NONE', #8340, #7867, #1067, .T. ) ;
#2073 = DIRECTION ( 'NONE',  ( -1.000000000000000000, -8.881784197001244435E-16, -0.000000000000000000 ) ) ;
#2074 = DIRECTION ( 'NONE',  ( 1.000000000000000000, -1.284024588418159550E-35, 0.000000000000000000 ) ) ;
#2075 = DIRECTION ( 'NONE',  ( 0.000000000000000000, 0.000000000000000000, 1.000000000000000000 ) ) ;
#2076 = PLANE ( 'NONE',  #4729 ) ;
#2077 = DIRECTION ( 'NONE',  ( 0.000000000000000000, 0.000000000000000000, -1.000000000000000000 ) ) ;
#2078 = EDGE_LOOP ( 'NONE', ( #6598, #229, #4268, #4956, #4753, #4271 ) ) ;
#2079 = CARTESIAN_POINT ( 'NONE',  ( -7.999999999999888978, 0.7809653281574794326, 6.859442213454772481E-14 ) ) ;
#2080 = ORIENTED_EDGE ( 'NONE', *, *, #559, .F. ) ;
#2081 = CIRCLE ( 'NONE', #1787, 3.309499999999999886 ) ;
#2082 = CIRCLE ( 'NONE', #2342, 5.500000000000000000 ) ;
#2083 = EDGE_CURVE ( 'NONE', #5384, #4294, #3684, .T. ) ;
#2084 = CARTESIAN_POINT ( 'NONE',  ( -1.313474075707264488, -8.479269695850916833, -0.3167204509598732787 ) ) ;
#2085 = CARTESIAN_POINT ( 'NONE',  ( 28.24999999999996803, 1.387778780781445676E-14, 1.504632769052525000E-32 ) ) ;
#2086 = CARTESIAN_POINT ( 'NONE',  ( 0.000000000000000000, 299.9999999999999432, -5.551115123125782702E-14 ) ) ;
#2087 = CONTEXT_DEPENDENT_SHAPE_REPRESENTATION ( #5060, #768 ) ;
#2088 = AXIS2_PLACEMENT_3D ( 'NONE', #3246, #58, #1285 ) ;
#2089 = CIRCLE ( 'NONE', #8200, 14.99999999999987388 ) ;
#2090 = CARTESIAN_POINT ( 'NONE',  ( -2.644994884459265005, 7.710515798486376582, -8.317753204360265329 ) ) ;
#2091 = AXIS2_PLACEMENT_3D ( 'NONE', #7338, #6604, #5389 ) ;
#2092 = CARTESIAN_POINT ( 'NONE',  ( -3.319543390096982183, 7.321065037175590540, -8.383111142571939567 ) ) ;
#2093 = VERTEX_POINT ( 'NONE', #3767 ) ;
#2094 = AXIS2_PLACEMENT_3D ( 'NONE', #7176, #2598, #8004 ) ;
#2095 = PRODUCT_DEFINITION_SHAPE ( 'NONE', 'NONE',  #8618 ) ;
#2096 = EDGE_LOOP ( 'NONE', ( #7375, #4336 ) ) ;
#2097 = PLANE ( 'NONE',  #164 ) ;
#2098 = VERTEX_POINT ( 'NONE', #458 ) ;
#2099 = CARTESIAN_POINT ( 'NONE',  ( -50.00000000000004263, 425.0000000000000000, -25.00000000000000355 ) ) ;
#2100 = AXIS2_PLACEMENT_3D ( 'NONE', #6199, #5587, #1556 ) ;
#2101 = CIRCLE ( 'NONE', #6813, 25.00000000000000711 ) ;
#2102 = CARTESIAN_POINT ( 'NONE',  ( -17.49999999999955236, 120.0000000000003268, 9.999999999999980460 ) ) ;
#2103 = CYLINDRICAL_SURFACE ( 'NONE', #3993, 5.499999999999999112 ) ;
#2104 = VECTOR ( 'NONE', #616, 1000.000000000000000 ) ;
#2105 = AXIS2_PLACEMENT_3D ( 'NONE', #1646, #2967, #261 ) ;
#2106 = ORIENTED_EDGE ( 'NONE', *, *, #5643, .T. ) ;
#2107 = DIRECTION ( 'NONE',  ( 1.000000000000000000, 0.000000000000000000, -6.938893903907228378E-17 ) ) ;
#2108 = ORIENTED_EDGE ( 'NONE', *, *, #3505, .F. ) ;
#2109 = ORIENTED_EDGE ( 'NONE', *, *, #1847, .F. ) ;
#2110 = AXIS2_PLACEMENT_3D ( 'NONE', #3460, #2803, #2846 ) ;
#2111 = COLOUR_RGB ( '',0.7921568627450980005, 0.8196078431372548767, 0.9333333333333333481 ) ;
#2112 = PRODUCT_DEFINITION_SHAPE ( 'NONE', 'NONE',  #8608 ) ;
#2113 = EDGE_CURVE ( 'NONE', #947, #2145, #1270, .T. ) ;
#2114 = CARTESIAN_POINT ( 'NONE',  ( -99.99999999999961631, 120.0000000000001137, 10.00000000000000888 ) ) ;
#2115 = AXIS2_PLACEMENT_3D ( 'NONE', #5322, #5185, #7322 ) ;
#2116 = ORIENTED_EDGE ( 'NONE', *, *, #7710, .F. ) ;
#2117 = CARTESIAN_POINT ( 'NONE',  ( 0.7999999999999674039, 7.960204194457039156E-16, 6.499999999999968026 ) ) ;
#2118 = ORIENTED_EDGE ( 'NONE', *, *, #3608, .F. ) ;
#2119 = EDGE_CURVE ( 'NONE', #6993, #6484, #5717, .T. ) ;
#2120 = PRODUCT_RELATED_PRODUCT_CATEGORY ( 'part', '', ( #5939 ) ) ;
#2121 = CARTESIAN_POINT ( 'NONE',  ( -49.99999999999963762, 87.50000000000035527, 9.999999999999786837 ) ) ;
#2122 = VERTEX_POINT ( 'NONE', #5877 ) ;
#2123 = PLANE ( 'NONE',  #7963 ) ;
#2124 = DIRECTION ( 'NONE',  ( 0.000000000000000000, 0.000000000000000000, 1.000000000000000000 ) ) ;
#2125 = ORIENTED_EDGE ( 'NONE', *, *, #2156, .T. ) ;
#2126 = CARTESIAN_POINT ( 'NONE',  ( 2.220446049250313081E-13, 9.237604307034075646, -7.685468820183672278 ) ) ;
#2127 = CARTESIAN_POINT ( 'NONE',  ( 10.00000000000000888, 0.000000000000000000, 4.440892098500626162E-13 ) ) ;
#2128 = FACE_OUTER_BOUND ( 'NONE', #4821, .T. ) ;
#2129 = AXIS2_PLACEMENT_3D ( 'NONE', #1915, #740, #6529 ) ;
#2130 = CARTESIAN_POINT ( 'NONE',  ( 4.339467034331248918, 6.732211846623394891, -1.598414698939908181E-14 ) ) ;
#2131 = VERTEX_POINT ( 'NONE', #5194 ) ;
#2132 = EDGE_CURVE ( 'NONE', #8150, #6642, #5440, .T. ) ;
#2133 = DIRECTION ( 'NONE',  ( 3.851859888774471706E-33, 1.232595164407830946E-32, 1.000000000000000000 ) ) ;
#2134 = ORIENTED_EDGE ( 'NONE', *, *, #2890, .T. ) ;
#2135 = CARTESIAN_POINT ( 'NONE',  ( 44.99999999999992895, 500.0000000000000000, 45.00000000000000711 ) ) ;
#2136 = DIRECTION ( 'NONE',  ( 1.000000000000000000, 3.083952846180994816E-15, -3.821045009664285742E-30 ) ) ;
#2137 = VECTOR ( 'NONE', #5924, 1000.000000000000000 ) ;
#2138 = DIRECTION ( 'NONE',  ( 3.851859888774471706E-33, -7.598173571352216173E-18, 1.000000000000000000 ) ) ;
#2139 = AXIS2_PLACEMENT_3D ( 'NONE', #4194, #2201, #4850 ) ;
#2140 = LINE ( 'NONE', #7448, #4017 ) ;
#2141 = DIRECTION ( 'NONE',  ( -1.555753819465285427E-60, 1.110768649713241713E-15, 1.000000000000000000 ) ) ;
#2142 = EDGE_LOOP ( 'NONE', ( #33, #1106, #248, #6182 ) ) ;
#2143 = EDGE_CURVE ( 'NONE', #7867, #749, #8052, .T. ) ;
#2144 = CARTESIAN_POINT ( 'NONE',  ( 0.000000000000000000, 0.000000000000000000, -8.400000000000018119 ) ) ;
#2145 = VERTEX_POINT ( 'NONE', #3185 ) ;
#2146 = VECTOR ( 'NONE', #4165, 1000.000000000000000 ) ;
#2147 = CARTESIAN_POINT ( 'NONE',  ( -4.000000000000114575, -6.928203230275542523, 0.000000000000000000 ) ) ;
#2148 = DIRECTION ( 'NONE',  ( 0.9237280213470678847, 0.3830490080632384942, 0.000000000000000000 ) ) ;
#2149 = LINE ( 'NONE', #2050, #4965 ) ;
#2150 = ORIENTED_EDGE ( 'NONE', *, *, #4088, .T. ) ;
#2151 = DIRECTION ( 'NONE',  ( 0.000000000000000000, 0.000000000000000000, 1.000000000000000000 ) ) ;
#2152 = ORIENTED_EDGE ( 'NONE', *, *, #7413, .T. ) ;
#2153 = ORIENTED_EDGE ( 'NONE', *, *, #2377, .F. ) ;
#2154 = VECTOR ( 'NONE', #7172, 1000.000000000000000 ) ;
#2155 = EDGE_CURVE ( 'NONE', #4565, #6245, #2101, .T. ) ;
#2156 = EDGE_CURVE ( 'NONE', #927, #7841, #1928, .T. ) ;
#2157 = APPLICATION_CONTEXT ( 'automotive_design' ) ;
#2158 = PRESENTATION_STYLE_ASSIGNMENT (( #5374 ) ) ;
#2159 = DIRECTION ( 'NONE',  ( 0.000000000000000000, 0.000000000000000000, 1.000000000000000000 ) ) ;
#2160 = AXIS2_PLACEMENT_3D ( 'NONE', #714, #3366, #45 ) ;
#2161 = EDGE_CURVE ( 'NONE', #4536, #8239, #6044, .T. ) ;
#2162 = ORIENTED_EDGE ( 'NONE', *, *, #4374, .F. ) ;
#2163 = DIRECTION ( 'NONE',  ( 1.000000000000000000, 2.715219353702835081E-15, -3.821045009664285041E-30 ) ) ;
#2164 = DIRECTION ( 'NONE',  ( -1.000000000000000000, 0.000000000000000000, 0.000000000000000000 ) ) ;
#2165 = ORIENTED_EDGE ( 'NONE', *, *, #8332, .T. ) ;
#2166 = ADVANCED_FACE ( 'NONE', ( #4634 ), #7846, .F. ) ;
#2167 = VERTEX_POINT ( 'NONE', #2624 ) ;
#2168 = DIRECTION ( 'NONE',  ( 3.919652622816902408E-30, 3.944304526105059027E-30, -1.000000000000000000 ) ) ;
#2169 = CIRCLE ( 'NONE', #911, 49.99999999999998579 ) ;
#2170 = CYLINDRICAL_SURFACE ( 'NONE', #3581, 15.00000000000000355 ) ;
#2171 = PRODUCT_DEFINITION_SHAPE ( 'NONE', 'NONE',  #8633 ) ;
#2172 = FACE_OUTER_BOUND ( 'NONE', #7634, .T. ) ;
#2173 = CARTESIAN_POINT ( 'NONE',  ( -49.99999999999953815, 120.0000000000003268, 9.999999999999980460 ) ) ;
#2174 = ORIENTED_EDGE ( 'NONE', *, *, #8270, .F. ) ;
#2175 = FACE_OUTER_BOUND ( 'NONE', #5707, .T. ) ;
#2176 = LINE ( 'NONE', #1509, #2146 ) ;
#2177 = CARTESIAN_POINT ( 'NONE',  ( 3.319543390095492263, -7.321065037175465307, -0.01688885742765811049 ) ) ;
#2178 = EDGE_CURVE ( 'NONE', #218, #303, #4541, .T. ) ;
#2179 = DIRECTION ( 'NONE',  ( 3.549874073494553124E-30, -0.5000000000000009992, -0.8660254037844380415 ) ) ;
#2180 = DIRECTION ( 'NONE',  ( -1.000000000000000000, 0.000000000000000000, 0.000000000000000000 ) ) ;
#2181 = ORIENTED_EDGE ( 'NONE', *, *, #4908, .T. ) ;
#2182 = VERTEX_POINT ( 'NONE', #7938 ) ;
#2183 = LINE ( 'NONE', #4137, #305 ) ;
#2184 = DIRECTION ( 'NONE',  ( -0.5000000000000044409, -7.442594376397861402E-30, 0.8660254037844360431 ) ) ;
#2185 = ADVANCED_FACE ( 'NONE', ( #3881 ), #1247, .T. ) ;
#2186 = ORIENTED_EDGE ( 'NONE', *, *, #4471, .T. ) ;
#2187 = CARTESIAN_POINT ( 'NONE',  ( -4.000000000000891731, 6.928203230275542523, -8.400000000000018119 ) ) ;
#2188 = ORIENTED_EDGE ( 'NONE', *, *, #6939, .T. ) ;
#2189 = ORIENTED_EDGE ( 'NONE', *, *, #2840, .T. ) ;
#2190 = CONICAL_SURFACE ( 'NONE', #7060, 4.057500000000000107, 1.047197551196592746 ) ;
#2191 = EDGE_CURVE ( 'NONE', #2020, #6788, #2382, .T. ) ;
#2192 = VERTEX_POINT ( 'NONE', #8117 ) ;
#2193 =( REPRESENTATION_RELATIONSHIP ('NONE','NONE', #1279, #5209 ) REPRESENTATION_RELATIONSHIP_WITH_TRANSFORMATION ( #1267 )SHAPE_REPRESENTATION_RELATIONSHIP( ) );
#2194 = EDGE_CURVE ( 'NONE', #6000, #3126, #6856, .T. ) ;
#2195 = CARTESIAN_POINT ( 'NONE',  ( -2.644994884459048290, 7.710515798486305528, -8.317753204360352370 ) ) ;
#2196 = CARTESIAN_POINT ( 'NONE',  ( -8.000000000000007105, 1.110223024625156540E-13, -8.400000000000018119 ) ) ;
#2197 = DIRECTION ( 'NONE',  ( 0.9237280213470682178, 0.3830490080632377725, 0.000000000000000000 ) ) ;
#2198 = ORIENTED_EDGE ( 'NONE', *, *, #3984, .T. ) ;
#2199 = CYLINDRICAL_SURFACE ( 'NONE', #8478, 24.49999999999999645 ) ;
#2200 = EDGE_LOOP ( 'NONE', ( #2301, #8458, #3544 ) ) ;
#2201 = DIRECTION ( 'NONE',  ( 1.463706757734299248E-32, -1.000000000000000000, -5.238529448733281520E-32 ) ) ;
#2202 = CARTESIAN_POINT ( 'NONE',  ( 0.000000000000000000, 60.00000000000000000, 50.00000000000000000 ) ) ;
#2203 = ORIENTED_EDGE ( 'NONE', *, *, #3116, .T. ) ;
#2204 = LINE ( 'NONE', #5565, #5002 ) ;
#2205 = CARTESIAN_POINT ( 'NONE',  ( -8.000000000000673239, 4.618802153517287401, -0.7145311798163467287 ) ) ;
#2206 = SHAPE_REPRESENTATION_RELATIONSHIP ( 'NONE' , 'NONE' ,  #5209, #230 ) ;
#2207 = EDGE_LOOP ( 'NONE', ( #549, #5563, #8384 ) ) ;
#2208 = ADVANCED_FACE ( 'NONE', ( #3543 ), #4063, .F. ) ;
#2209 = CARTESIAN_POINT ( 'NONE',  ( -7.347286611336995676, -4.995646404165323240, -7.903039949738239756 ) ) ;
#2210 = CARTESIAN_POINT ( 'NONE',  ( 8.000000000000229150, -1.665334536937734811E-13, -8.400000000000018119 ) ) ;
#2211 = DIRECTION ( 'NONE',  ( 0.000000000000000000, -5.322451846059954622E-30, 1.000000000000000000 ) ) ;
#2212 = CARTESIAN_POINT ( 'NONE',  ( 5.354491962338145505, -6.146186931204510984, -8.331901280394534481 ) ) ;
#2213 = DIRECTION ( 'NONE',  ( 0.000000000000000000, -5.322451846059954622E-30, 1.000000000000000000 ) ) ;
#2214 = VERTEX_POINT ( 'NONE', #6727 ) ;
#2215 = CARTESIAN_POINT ( 'NONE',  ( 0.000000000000000000, 0.000000000000000000, 0.000000000000000000 ) ) ;
#2216 = VERTEX_POINT ( 'NONE', #3412 ) ;
#2217 = EDGE_CURVE ( 'NONE', #6543, #462, #3178, .T. ) ;
#2218 = PRODUCT_RELATED_PRODUCT_CATEGORY ( 'part', '', ( #5872 ) ) ;
#2219 = LINE ( 'NONE', #3527, #4211 ) ;
#2220 = DIRECTION ( 'NONE',  ( -1.000000000000000000, 1.774937036747276562E-30, 0.000000000000000000 ) ) ;
#2221 = VERTEX_POINT ( 'NONE', #6776 ) ;
#2222 = DIRECTION ( 'NONE',  ( -6.938893903907228378E-17, 0.000000000000000000, -1.000000000000000000 ) ) ;
#2223 = ORIENTED_EDGE ( 'NONE', *, *, #3549, .T. ) ;
#2224 = VECTOR ( 'NONE', #5858, 1000.000000000000000 ) ;
#2225 = ORIENTED_EDGE ( 'NONE', *, *, #5179, .F. ) ;
#2226 = EDGE_CURVE ( 'NONE', #8239, #3300, #5651, .T. ) ;
#2227 = CARTESIAN_POINT ( 'NONE',  ( 275.0000000000000000, 425.0000000000000000, 75.00000000000015632 ) ) ;
#2228 =( REPRESENTATION_RELATIONSHIP ('NONE','NONE', #1279, #1942 ) REPRESENTATION_RELATIONSHIP_WITH_TRANSFORMATION ( #7139 )SHAPE_REPRESENTATION_RELATIONSHIP( ) );
#2229=STYLED_ITEM('',(#8670),#2980);
#2230 = ORIENTED_EDGE ( 'NONE', *, *, #3361, .T. ) ;
#2231 = CYLINDRICAL_SURFACE ( 'NONE', #5281, 25.00000000000000711 ) ;
#2232 = CIRCLE ( 'NONE', #7106, 25.00000000000000711 ) ;
#2233 = DIRECTION ( 'NONE',  ( 1.000000000000000000, -5.898059818321126865E-17, -4.579669976578766785E-16 ) ) ;
#2234 = ORIENTED_EDGE ( 'NONE', *, *, #1808, .T. ) ;
#2235 = B_SPLINE_CURVE_WITH_KNOTS ( 'NONE', 3,
 ( #4881, #921, #6291, #1605, #7496, #2187 ),
 .UNSPECIFIED., .F., .F.,
 ( 4, 2, 4 ),
 ( 2.380731626810059357E-07, 0.002336973833157153079, 0.004673709593151625756 ),
 .UNSPECIFIED. ) ;
#2236 = CARTESIAN_POINT ( 'NONE',  ( -4.000000000000003553, 6.928203230275209457, -8.400000000000018119 ) ) ;
#2237 = ADVANCED_FACE ( 'NONE', ( #1059 ), #4036, .T. ) ;
#2238 = ORIENTED_EDGE ( 'NONE', *, *, #7447, .F. ) ;
#2239 = CARTESIAN_POINT ( 'NONE',  ( 4.000000000000003553, -6.928203230275542523, -8.400000000000018119 ) ) ;
#2240 = DIRECTION ( 'NONE',  ( 0.000000000000000000, 0.000000000000000000, 1.000000000000000000 ) ) ;
#2241 = DIRECTION ( 'NONE',  ( 3.851859888774471706E-33, 1.232595164407830946E-32, 1.000000000000000000 ) ) ;
#2242 = ORIENTED_EDGE ( 'NONE', *, *, #3280, .F. ) ;
#2243 = CARTESIAN_POINT ( 'NONE',  ( 0.000000000000000000, 0.000000000000000000, -10.00000000000006395 ) ) ;
#2244 = DIRECTION ( 'NONE',  ( -3.919652622816902408E-30, -3.944304526105059027E-30, 1.000000000000000000 ) ) ;
#2245 = ORIENTED_EDGE ( 'NONE', *, *, #5821, .F. ) ;
#2246 = ADVANCED_FACE ( 'NONE', ( #2348 ), #1401, .T. ) ;
#2247 = CYLINDRICAL_SURFACE ( 'NONE', #8107, 75.00000000000005684 ) ;
#2248 = EDGE_LOOP ( 'NONE', ( #6424, #4523 ) ) ;
#2249 = ORIENTED_EDGE ( 'NONE', *, *, #5574, .T. ) ;
#2250 = EDGE_CURVE ( 'NONE', #4067, #5769, #5139, .T. ) ;
#2251 = CARTESIAN_POINT ( 'NONE',  ( 5.499999999999999112, 60.00000000000000000, -50.00000000000000000 ) ) ;
#2252=STYLED_ITEM('',(#8677),#132);
#2253 = DIRECTION ( 'NONE',  ( -3.919652622816902408E-30, -3.944304526105059027E-30, 1.000000000000000000 ) ) ;
#2254 = DIRECTION ( 'NONE',  ( -0.7071067811864683028, -2.508471778025259936E-30, 0.7071067811866268427 ) ) ;
#2255 = DIRECTION ( 'NONE',  ( 3.919652622816902408E-30, 3.944304526105059027E-30, -1.000000000000000000 ) ) ;
#2256 = PLANE ( 'NONE',  #6146 ) ;
#2257 = EDGE_LOOP ( 'NONE', ( #2795, #7341, #6442, #2605 ) ) ;
#2258 = CARTESIAN_POINT ( 'NONE',  ( 2.644994884458967910, -7.710515798486506256, -0.08224679563976267094 ) ) ;
#2259 = EDGE_LOOP ( 'NONE', ( #8257, #2990 ) ) ;
#2260 = EDGE_CURVE ( 'NONE', #2221, #2870, #1231, .T. ) ;
#2261 = AXIS2_PLACEMENT_3D ( 'NONE', #7188, #5267, #6624 ) ;
#2262 = AXIS2_PLACEMENT_3D ( 'NONE', #5573, #4085, #6270 ) ;
#2263 = FACE_OUTER_BOUND ( 'NONE', #1122, .T. ) ;
#2264 = VERTEX_POINT ( 'NONE', #492 ) ;
#2265 = CARTESIAN_POINT ( 'NONE',  ( -32.49999999999997158, 3.469446951953614189E-15, 18.00000000000000355 ) ) ;
#2266 = ORIENTED_EDGE ( 'NONE', *, *, #7511, .F. ) ;
#2267 = VECTOR ( 'NONE', #1844, 1000.000000000000000 ) ;
#2268 = ORIENTED_EDGE ( 'NONE', *, *, #8323, .T. ) ;
#2269 = CIRCLE ( 'NONE', #1694, 6.500000000000002665 ) ;
#2270 = AXIS2_PLACEMENT_3D ( 'NONE', #6878, #8175, #4906 ) ;
#2271 = AXIS2_PLACEMENT_3D ( 'NONE', #4493, #7984, #4632 ) ;
#2272 = DIRECTION ( 'NONE',  ( -3.451266460341926211E-31, 0.4999999999999985567, -0.8660254037844393737 ) ) ;
#2273 = ADVANCED_FACE ( 'NONE', ( #1781 ), #3757, .F. ) ;
#2274 = ORIENTED_EDGE ( 'NONE', *, *, #4833, .F. ) ;
#2275 = DIRECTION ( 'NONE',  ( 1.000000000000000000, 3.083952846180997183E-15, 0.000000000000000000 ) ) ;
#2276 = DIRECTION ( 'NONE',  ( -1.000000000000000000, 0.000000000000000000, 0.000000000000000000 ) ) ;
#2277 = DIRECTION ( 'NONE',  ( 0.000000000000000000, 0.000000000000000000, 1.000000000000000000 ) ) ;
#2278 = VERTEX_POINT ( 'NONE', #6380 ) ;
#2279 = DIRECTION ( 'NONE',  ( 1.000000000000000000, 0.000000000000000000, 0.000000000000000000 ) ) ;
#2280 = ORIENTED_EDGE ( 'NONE', *, *, #7249, .T. ) ;
#2281 = FACE_OUTER_BOUND ( 'NONE', #8118, .T. ) ;
#2282 =( GEOMETRIC_REPRESENTATION_CONTEXT ( 3 ) GLOBAL_UNCERTAINTY_ASSIGNED_CONTEXT ( ( #8368 ) ) GLOBAL_UNIT_ASSIGNED_CONTEXT ( ( #4544, #4499, #5198 ) ) REPRESENTATION_CONTEXT ( 'NONE', 'WORKASPACE' ) );
#2283 = DIRECTION ( 'NONE',  ( -3.919652622816902408E-30, -3.944304526105059027E-30, 1.000000000000000000 ) ) ;
#2284 = PLANE ( 'NONE',  #6650 ) ;
#2285 = EDGE_CURVE ( 'NONE', #2701, #3620, #404, .T. ) ;
#2286 = ORIENTED_EDGE ( 'NONE', *, *, #8009, .F. ) ;
#2287 = CARTESIAN_POINT ( 'NONE',  ( 8.000000000000007105, 4.618802153516732290, -0.7145311798163467287 ) ) ;
#2288 = AXIS2_PLACEMENT_3D ( 'NONE', #2405, #3060, #6343 ) ;
#2289 = CIRCLE ( 'NONE', #2851, 4.499999999999997335 ) ;
#2290 = VERTEX_POINT ( 'NONE', #3054 ) ;
#2291 = ORIENTED_EDGE ( 'NONE', *, *, #1747, .F. ) ;
#2292 = CARTESIAN_POINT ( 'NONE',  ( 0.000000000000000000, 0.000000000000000000, 5.551115123125782702E-14 ) ) ;
#2293 = CARTESIAN_POINT ( 'NONE',  ( 5.354491962338240540, -6.146186931204690396, -8.331901280394420795 ) ) ;
#2294 = ADVANCED_FACE ( 'NONE', ( #2312 ), #7081, .T. ) ;
#2295 = FACE_OUTER_BOUND ( 'NONE', #755, .T. ) ;
#2296 = DIRECTION ( 'NONE',  ( 0.000000000000000000, 0.000000000000000000, 1.000000000000000000 ) ) ;
#2297 = DIRECTION ( 'NONE',  ( 0.000000000000000000, 0.000000000000000000, -1.000000000000000000 ) ) ;
#2298 = ORIENTED_EDGE ( 'NONE', *, *, #6981, .T. ) ;
#2299 = B_SPLINE_CURVE_WITH_KNOTS ( 'NONE', 3,
 ( #2042, #4704, #4046, #6706, #735, #6070 ),
 .UNSPECIFIED., .F., .F.,
 ( 4, 2, 4 ),
 ( 0.01291313371729494418, 0.01525081363757336758, 0.01758849355785178925 ),
 .UNSPECIFIED. ) ;
#2300 = FACE_BOUND ( 'NONE', #6674, .T. ) ;
#2301 = ORIENTED_EDGE ( 'NONE', *, *, #494, .T. ) ;
#2302 = CIRCLE ( 'NONE', #5667, 24.50000000000000000 ) ;
#2303 = LINE ( 'NONE', #2834, #38 ) ;
#2304 = FACE_OUTER_BOUND ( 'NONE', #7, .T. ) ;
#2305 = VERTEX_POINT ( 'NONE', #5824 ) ;
#2306 = VECTOR ( 'NONE', #2824, 1000.000000000000000 ) ;
#2307 = EDGE_LOOP ( 'NONE', ( #1322, #4419 ) ) ;
#2308 = DIRECTION ( 'NONE',  ( -3.851859888774471706E-33, 7.598173571352185358E-18, -1.000000000000000000 ) ) ;
#2309 = SURFACE_SIDE_STYLE ('',( #8284 ) ) ;
#2310 = CIRCLE ( 'NONE', #1892, 4.499999999999993783 ) ;
#2311 = FACE_OUTER_BOUND ( 'NONE', #3636, .T. ) ;
#2312 = FACE_OUTER_BOUND ( 'NONE', #640, .T. ) ;
#2313 = VERTEX_POINT ( 'NONE', #5784 ) ;
#2314 = CARTESIAN_POINT ( 'NONE',  ( 2.644994884459147766, -7.710515798486462735, -8.317753204360245789 ) ) ;
#2315 = CIRCLE ( 'NONE', #3842, 4.499999999999990230 ) ;
#2316 = CARTESIAN_POINT ( 'NONE',  ( -5.354491962338013167, 6.146186931204386639, -8.331901280394641063 ) ) ;
#2317 = ORIENTED_EDGE ( 'NONE', *, *, #2619, .T. ) ;
#2318 = PLANE ( 'NONE',  #3189 ) ;
#2319 = ORIENTED_EDGE ( 'NONE', *, *, #1993, .T. ) ;
#2320 = CARTESIAN_POINT ( 'NONE',  ( 0.000000000000000000, 0.000000000000000000, -109.9999999999999574 ) ) ;
#2321 = EDGE_CURVE ( 'NONE', #7532, #173, #259, .T. ) ;
#2322 = DIRECTION ( 'NONE',  ( -1.000000000000000000, 3.549874073494553124E-30, 0.000000000000000000 ) ) ;
#2323 = ORIENTED_EDGE ( 'NONE', *, *, #7306, .F. ) ;
#2324 = DIRECTION ( 'NONE',  ( 0.000000000000000000, -5.322451846059954622E-30, 1.000000000000000000 ) ) ;
#2325 =( LENGTH_UNIT ( ) NAMED_UNIT ( * ) SI_UNIT ( .MILLI., .METRE. ) );
#2326 = ORIENTED_EDGE ( 'NONE', *, *, #4473, .F. ) ;
#2327 = FACE_OUTER_BOUND ( 'NONE', #8408, .T. ) ;
#2328 = ORIENTED_EDGE ( 'NONE', *, *, #1794, .F. ) ;
#2329 = ORIENTED_EDGE ( 'NONE', *, *, #8279, .F. ) ;
#2330 = DIRECTION ( 'NONE',  ( -1.000000000000000000, 3.549874073494553124E-30, -0.000000000000000000 ) ) ;
#2331 = EDGE_CURVE ( 'NONE', #6484, #1589, #688, .T. ) ;
#2332 = FACE_OUTER_BOUND ( 'NONE', #3534, .T. ) ;
#2333 =( NAMED_UNIT ( * ) PLANE_ANGLE_UNIT ( ) SI_UNIT ( $, .RADIAN. ) );
#2334 = CARTESIAN_POINT ( 'NONE',  ( -12.99999999999957723, 120.0000000000003411, 1.763843680267613651E-29 ) ) ;
#2335 = FACE_OUTER_BOUND ( 'NONE', #3132, .T. ) ;
#2336 = VERTEX_POINT ( 'NONE', #8417 ) ;
#2337 = CARTESIAN_POINT ( 'NONE',  ( 4.000000000000003553, -6.928203230275542523, 0.000000000000000000 ) ) ;
#2338 = VERTEX_POINT ( 'NONE', #6941 ) ;
#2339 = EDGE_CURVE ( 'NONE', #5854, #2009, #6338, .T. ) ;
#2340 = DIRECTION ( 'NONE',  ( 6.400024471206996205E-36, -1.000000000000000000, -7.598173571352216173E-18 ) ) ;
#2341 = DIRECTION ( 'NONE',  ( 0.000000000000000000, 0.000000000000000000, 1.000000000000000000 ) ) ;
#2342 = AXIS2_PLACEMENT_3D ( 'NONE', #3203, #8511, #5159 ) ;
#2343 = B_SPLINE_CURVE_WITH_KNOTS ( 'NONE', 3,
 ( #7443, #1508, #7741, #1773, #3786, #6814, #842, #1363 ),
 .UNSPECIFIED., .F., .F.,
 ( 4, 2, 2, 4 ),
 ( 0.004673709593152015201, 0.005837709341827571410, 0.007001709090503128487, 0.009329708587854243507 ),
 .UNSPECIFIED. ) ;
#2344 = EDGE_LOOP ( 'NONE', ( #6733, #905, #8425, #1309, #3615 ) ) ;
#2345 = APPLICATION_CONTEXT ( 'automotive_design' ) ;
#2346 = UNCERTAINTY_MEASURE_WITH_UNIT (LENGTH_MEASURE( 1.000000000000000082E-05 ), #5167, 'distance_accuracy_value', 'NONE');
#2347 = DIRECTION ( 'NONE',  ( 0.000000000000000000, 0.000000000000000000, -1.000000000000000000 ) ) ;
#2348 = FACE_OUTER_BOUND ( 'NONE', #8086, .T. ) ;
#2349 = VERTEX_POINT ( 'NONE', #970 ) ;
#2350 = CIRCLE ( 'NONE', #6531, 69.99999999999998579 ) ;
#2351 = CARTESIAN_POINT ( 'NONE',  ( 2.694222958124174048E-15, 415.0000000000000000, 19.49999999999990763 ) ) ;
#2352 = CARTESIAN_POINT ( 'NONE',  ( -49.99999999999954525, 120.0000000000003268, 0.000000000000000000 ) ) ;
#2353 = SHAPE_DEFINITION_REPRESENTATION ( #7095, #3455 ) ;
#2354 = VECTOR ( 'NONE', #2732, 1000.000000000000000 ) ;
#2355 = DIRECTION ( 'NONE',  ( -3.851859888774471706E-33, 7.598173571352223877E-18, -1.000000000000000000 ) ) ;
#2356 = CIRCLE ( 'NONE', #8206, 25.00000000000000711 ) ;
#2357 = VECTOR ( 'NONE', #7940, 1000.000000000000000 ) ;
#2358 = FACE_OUTER_BOUND ( 'NONE', #2257, .T. ) ;
#2359 = VECTOR ( 'NONE', #8298, 1000.000000000000000 ) ;
#2360 = COLOUR_RGB ( '',0.7921568627450980005, 0.8196078431372548767, 0.9333333333333333481 ) ;
#2361 = LINE ( 'NONE', #7639, #2490 ) ;
#2362 = EDGE_LOOP ( 'NONE', ( #5266, #2365, #7513 ) ) ;
#2363 = AXIS2_PLACEMENT_3D ( 'NONE', #5654, #1137, #3798 ) ;
#2364 = PLANE ( 'NONE',  #7093 ) ;
#2365 = ORIENTED_EDGE ( 'NONE', *, *, #6226, .T. ) ;
#2366 = VECTOR ( 'NONE', #2909, 1000.000000000000000 ) ;
#2367 = ORIENTED_EDGE ( 'NONE', *, *, #632, .T. ) ;
#2368 = FACE_BOUND ( 'NONE', #7739, .T. ) ;
#2369 = VERTEX_POINT ( 'NONE', #3635 ) ;
#2370 = CIRCLE ( 'NONE', #4607, 10.49999999999999645 ) ;
#2371 = CYLINDRICAL_SURFACE ( 'NONE', #5767, 25.00000000000000711 ) ;
#2372 = AXIS2_PLACEMENT_3D ( 'NONE', #8142, #2141, #6662 ) ;
#2373 = PRODUCT_DEFINITION_CONTEXT ( 'detailed design', #8581, 'design' ) ;
#2374 = DIRECTION ( 'NONE',  ( 0.000000000000000000, 0.000000000000000000, -1.000000000000000000 ) ) ;
#2375 = SURFACE_STYLE_FILL_AREA ( #8351 ) ;
#2376 = DIRECTION ( 'NONE',  ( 3.919652622816902408E-30, 3.944304526105059027E-30, -1.000000000000000000 ) ) ;
#2377 = EDGE_CURVE ( 'NONE', #5689, #3300, #4968, .T. ) ;
#2378 = DIRECTION ( 'NONE',  ( 1.000000000000000000, -3.549874073494553124E-30, 0.000000000000000000 ) ) ;
#2379 = EDGE_LOOP ( 'NONE', ( #1555, #6607 ) ) ;
#2380 = DIRECTION ( 'NONE',  ( 6.400024471206996205E-36, -1.000000000000000000, -7.598173571352216173E-18 ) ) ;
#2381 = ORIENTED_EDGE ( 'NONE', *, *, #3717, .F. ) ;
#2382 = B_SPLINE_CURVE_WITH_KNOTS ( 'NONE', 3,
 ( #8244, #4718, #7418, #6213, #4185, #7371 ),
 .UNSPECIFIED., .F., .F.,
 ( 4, 2, 4 ),
 ( 0.008240550023493572671, 0.01057684187039396873, 0.01291313371729436651 ),
 .UNSPECIFIED. ) ;
#2383 = AXIS2_PLACEMENT_3D ( 'NONE', #5965, #8595, #5207 ) ;
#2384 = CARTESIAN_POINT ( 'NONE',  ( 0.000000000000000000, 299.9999999999999432, -6.938893903907228378E-14 ) ) ;
#2385 = CONTEXT_DEPENDENT_SHAPE_REPRESENTATION ( #4414, #778 ) ;
#2386 = EDGE_CURVE ( 'NONE', #316, #7714, #541, .T. ) ;
#2387 = DIRECTION ( 'NONE',  ( 3.851859888774471706E-33, -7.598173571352216173E-18, 1.000000000000000000 ) ) ;
#2388 = ORIENTED_EDGE ( 'NONE', *, *, #985, .T. ) ;
#2389 = ADVANCED_FACE ( 'NONE', ( #4498 ), #6500, .T. ) ;
#2390 = VERTEX_POINT ( 'NONE', #5066 ) ;
#2391 =( REPRESENTATION_RELATIONSHIP ('NONE','NONE', #1279, #6969 ) REPRESENTATION_RELATIONSHIP_WITH_TRANSFORMATION ( #5978 )SHAPE_REPRESENTATION_RELATIONSHIP( ) );
#2392 = CIRCLE ( 'NONE', #6443, 25.00000000000000711 ) ;
#2393 = VECTOR ( 'NONE', #719, 1000.000000000000000 ) ;
#2394 = CYLINDRICAL_SURFACE ( 'NONE', #4225, 5.500000000000023981 ) ;
#2395 = EDGE_CURVE ( 'NONE', #4021, #2167, #7762, .T. ) ;
#2396 = AXIS2_PLACEMENT_3D ( 'NONE', #1280, #7852, #1888 ) ;
#2397 = SHAPE_REPRESENTATION ( 'hex nut style 1_am_B18.2.4.1M - Hex nut, Style 1,  M10 x 1.5, with 16mm WAF --D-N', ( #7563 ), #3397 ) ;
#2398 = DIRECTION ( 'NONE',  ( 6.938893903907228378E-17, 0.000000000000000000, 1.000000000000000000 ) ) ;
#2399 = DIRECTION ( 'NONE',  ( 0.000000000000000000, -1.213383262747659708E-29, 1.000000000000000000 ) ) ;
#2400 = ORIENTED_EDGE ( 'NONE', *, *, #4919, .T. ) ;
#2401 = EDGE_CURVE ( 'NONE', #1795, #799, #2584, .T. ) ;
#2402 = AXIS2_PLACEMENT_3D ( 'NONE', #4004, #4668, #7922 ) ;
#2403 = CARTESIAN_POINT ( 'NONE',  ( 3.319543390096077129, -7.321065037175521262, -8.383111142572191810 ) ) ;
#2404 = DIRECTION ( 'NONE',  ( -3.919652622816902408E-30, -3.944304526105059027E-30, 1.000000000000000000 ) ) ;
#2405 = CARTESIAN_POINT ( 'NONE',  ( 422.5000000000001705, 29.99999999999845812, 67.99999999999991473 ) ) ;
#2406 = CIRCLE ( 'NONE', #598, 4.057500000000000107 ) ;
#2407 = CARTESIAN_POINT ( 'NONE',  ( 8.400000000000018119, 4.898587196541454030E-16, -3.999999999999364508 ) ) ;
#2408 = ADVANCED_FACE ( 'NONE', ( #577 ), #7504, .T. ) ;
#2409 = VECTOR ( 'NONE', #1320, 1000.000000000000000 ) ;
#2410 = CIRCLE ( 'NONE', #2972, 40.00000000000007816 ) ;
#2411 = CARTESIAN_POINT ( 'NONE',  ( -6.661338147750939243E-13, 9.237604307034352757, -8.400000000000018119 ) ) ;
#2412 = ORIENTED_EDGE ( 'NONE', *, *, #3154, .F. ) ;
#2413 = CARTESIAN_POINT ( 'NONE',  ( 1.110223024625156540E-13, -410.0000000000000568, -6.938893903907228378E-14 ) ) ;
#2414 = ORIENTED_EDGE ( 'NONE', *, *, #2717, .T. ) ;
#2415 = CIRCLE ( 'NONE', #2819, 8.000000000000007105 ) ;
#2416 = DIRECTION ( 'NONE',  ( 2.842664852890546338E-35, -1.000000000000000000, 0.000000000000000000 ) ) ;
#2417 = ORIENTED_EDGE ( 'NONE', *, *, #2820, .F. ) ;
#2418 = CARTESIAN_POINT ( 'NONE',  ( -2.300000000000024247, 0.000000000000000000, 5.559999999999998721 ) ) ;
#2419 = EDGE_CURVE ( 'NONE', #1055, #662, #691, .T. ) ;
#2420 = LINE ( 'NONE', #7082, #6730 ) ;
#2421 = CARTESIAN_POINT ( 'NONE',  ( -5.080504117408895404, -2.106769544347820933, 0.000000000000000000 ) ) ;
#2422 = CARTESIAN_POINT ( 'NONE',  ( -3.999999999999781508, -6.928203230275875590, 0.000000000000000000 ) ) ;
#2423 = DIRECTION ( 'NONE',  ( 0.000000000000000000, 0.000000000000000000, 1.000000000000000000 ) ) ;
#2424 = CARTESIAN_POINT ( 'NONE',  ( 0.000000000000000000, 60.00000000000000000, 45.00000000000000000 ) ) ;
#2425 = DIRECTION ( 'NONE',  ( -3.549874073494553124E-30, 1.000000000000000000, -8.626909098572831859E-16 ) ) ;
#2426 = CARTESIAN_POINT ( 'NONE',  ( -2.644994884458948814, 7.710515798486379246, -8.317753204360325725 ) ) ;
#2427 = ORIENTED_EDGE ( 'NONE', *, *, #5571, .F. ) ;
#2428 = CARTESIAN_POINT ( 'NONE',  ( 0.000000000000000000, 0.000000000000000000, 0.000000000000000000 ) ) ;
#2429 = ORIENTED_EDGE ( 'NONE', *, *, #1584, .F. ) ;
#2430 = CARTESIAN_POINT ( 'NONE',  ( 4.059252933785728601E-13, 119.9999999999998863, 10.00000000000000888 ) ) ;
#2431 = ADVANCED_FACE ( 'NONE', ( #3932 ), #4730, .T. ) ;
#2432 = DIRECTION ( 'NONE',  ( -1.000000000000000000, -8.881784197001244435E-16, 0.000000000000000000 ) ) ;
#2433 = DIRECTION ( 'NONE',  ( 0.000000000000000000, 0.000000000000000000, -1.000000000000000000 ) ) ;
#2434 = EDGE_LOOP ( 'NONE', ( #2417, #1376, #8490, #6841 ) ) ;
#2435 = ORIENTED_EDGE ( 'NONE', *, *, #3681, .F. ) ;
#2436 = DIRECTION ( 'NONE',  ( 6.400024471206993532E-36, -1.000000000000000000, -7.598173571352213092E-18 ) ) ;
#2437 = EDGE_CURVE ( 'NONE', #3262, #4756, #8066, .T. ) ;
#2438 = CYLINDRICAL_SURFACE ( 'NONE', #1448, 25.00000000000000711 ) ;
#2439 = CONICAL_SURFACE ( 'NONE', #1886, 50.00000000000008527, 0.7853981633974497223 ) ;
#2440 = CARTESIAN_POINT ( 'NONE',  ( 9.999999999999896971, 0.000000000000000000, 79.99999999999995737 ) ) ;
#2441 = DIRECTION ( 'NONE',  ( 0.000000000000000000, 0.000000000000000000, 1.000000000000000000 ) ) ;
#2442 = ORIENTED_EDGE ( 'NONE', *, *, #1634, .T. ) ;
#2443 = CARTESIAN_POINT ( 'NONE',  ( 32.30950000000065359, -4.257395394114627200E-29, 4.000000000006943779 ) ) ;
#2444 = CARTESIAN_POINT ( 'NONE',  ( 1.310872448938031010, -8.480771745766503500, -8.082649155111303330 ) ) ;
#2445 = CARTESIAN_POINT ( 'NONE',  ( 7.345652830558639046, -4.996589667937789692, -0.4964154566688734338 ) ) ;
#2446 = PRODUCT_CONTEXT ( 'NONE', #1786, 'mechanical' ) ;
#2447 = ADVANCED_FACE ( 'NONE', ( #2675 ), #266, .T. ) ;
#2448 = AXIS2_PLACEMENT_3D ( 'NONE', #1994, #4561, #2518 ) ;
#2449 = DIRECTION ( 'NONE',  ( 0.000000000000000000, 0.000000000000000000, 1.000000000000000000 ) ) ;
#2450 = ORIENTED_EDGE ( 'NONE', *, *, #1562, .T. ) ;
#2451 = B_SPLINE_CURVE_WITH_KNOTS ( 'NONE', 3,
 ( #2064, #4721, #2583, #6002, #7290, #1414 ),
 .UNSPECIFIED., .F., .F.,
 ( 4, 2, 4 ),
 ( 2.380731633596903170E-07, 0.002336973833157671328, 0.004673709593151983109 ),
 .UNSPECIFIED. ) ;
#2452 = DIRECTION ( 'NONE',  ( -4.440892098500626951E-15, 0.000000000000000000, -1.000000000000000000 ) ) ;
#2453 = CARTESIAN_POINT ( 'NONE',  ( 139.1719999999995423, 3.469446951953633753E-14, -1.443289932012703503E-12 ) ) ;
#2454 = EDGE_LOOP ( 'NONE', ( #3882, #6076, #7466 ) ) ;
#2455 = DIRECTION ( 'NONE',  ( -1.000000000000000000, -8.881784197001244435E-16, 0.000000000000000000 ) ) ;
#2456 = EDGE_LOOP ( 'NONE', ( #7051, #6209, #1816, #594 ) ) ;
#2457 = PLANE ( 'NONE',  #6567 ) ;
#2458 = CIRCLE ( 'NONE', #6798, 8.000000000000007105 ) ;
#2459 = FACE_OUTER_BOUND ( 'NONE', #1147, .T. ) ;
#2460 = DIRECTION ( 'NONE',  ( 1.000000000000000000, 8.881784197001244435E-16, 0.000000000000000000 ) ) ;
#2461 = LINE ( 'NONE', #5112, #7266 ) ;
#2462 = DIRECTION ( 'NONE',  ( -1.000000000000000000, -8.881784197001244435E-16, 0.000000000000000000 ) ) ;
#2463 = CYLINDRICAL_SURFACE ( 'NONE', #8529, 6.500000000000001776 ) ;
#2464 = EDGE_LOOP ( 'NONE', ( #435, #913, #7619, #4674, #7990, #405 ) ) ;
#2465 = ADVANCED_FACE ( 'NONE', ( #7507 ), #7590, .T. ) ;
#2466 = EDGE_CURVE ( 'NONE', #1391, #5417, #2350, .T. ) ;
#2467 = VERTEX_POINT ( 'NONE', #8202 ) ;
#2468 = DIRECTION ( 'NONE',  ( 0.000000000000000000, 1.000000000000000000, 1.795949010423047374E-16 ) ) ;
#2469 = ITEM_DEFINED_TRANSFORMATION ( 'NONE', 'NONE', #5496,  #7563 ) ;
#2470 = CARTESIAN_POINT ( 'NONE',  ( 15.50000000000011191, -14.99999999999990230, -20.00000000000001776 ) ) ;
#2471 = ORIENTED_EDGE ( 'NONE', *, *, #2395, .F. ) ;
#2472 = ORIENTED_EDGE ( 'NONE', *, *, #1979, .T. ) ;
#2473 = CARTESIAN_POINT ( 'NONE',  ( 0.000000000000000000, 0.000000000000000000, -8.400000000000018119 ) ) ;
#2474 = EDGE_CURVE ( 'NONE', #6426, #8386, #6945, .T. ) ;
#2475 = EDGE_CURVE ( 'NONE', #4132, #1579, #932, .T. ) ;
#2476 = ORIENTED_EDGE ( 'NONE', *, *, #5969, .T. ) ;
#2477 = AXIS2_PLACEMENT_3D ( 'NONE', #1775, #7223, #3788 ) ;
#2478 = DIRECTION ( 'NONE',  ( 0.000000000000000000, 0.000000000000000000, -1.000000000000000000 ) ) ;
#2479 = DIRECTION ( 'NONE',  ( 0.000000000000000000, -5.322451846059955323E-30, 1.000000000000000000 ) ) ;
#2480 = DIRECTION ( 'NONE',  ( -1.000000000000000000, -8.881784197001244435E-16, 0.000000000000000000 ) ) ;
#2481 = CARTESIAN_POINT ( 'NONE',  ( 0.000000000000000000, 0.000000000000000000, 0.000000000000000000 ) ) ;
#2482 = ORIENTED_EDGE ( 'NONE', *, *, #2561, .F. ) ;
#2483 = DIRECTION ( 'NONE',  ( 0.000000000000000000, -1.064348848528640545E-29, 1.000000000000000000 ) ) ;
#2484 = CARTESIAN_POINT ( 'NONE',  ( 0.000000000000000000, -9.237604307034075646, -7.685468820183672278 ) ) ;
#2485 = EDGE_CURVE ( 'NONE', #92, #1627, #6350, .T. ) ;
#2486 = AXIS2_PLACEMENT_3D ( 'NONE', #6799, #6233, #825 ) ;
#2487 = CARTESIAN_POINT ( 'NONE',  ( -7.345652830558607960, 4.996589667937374912, -7.903584543331300338 ) ) ;
#2488 = APPLICATION_PROTOCOL_DEFINITION ( 'draft international standard', 'automotive_design', 1998, #6817 ) ;
#2489 = CIRCLE ( 'NONE', #7501, 25.00000000000000711 ) ;
#2490 = VECTOR ( 'NONE', #3020, 1000.000000000000000 ) ;
#2491 = CIRCLE ( 'NONE', #7361, 50.00000000000008527 ) ;
#2492 = CARTESIAN_POINT ( 'NONE',  ( 4.000000000000058620, 3.518949890710762585, 2.220446049250313081E-13 ) ) ;
#2493 = EDGE_LOOP ( 'NONE', ( #1416, #2450, #5558, #521, #1455 ) ) ;
#2494 = B_SPLINE_CURVE_WITH_KNOTS ( 'NONE', 3,
 ( #6192, #3436, #200, #2293, #5626, #4949 ),
 .UNSPECIFIED., .F., .F.,
 ( 4, 2, 4 ),
 ( 2.380731633751139929E-07, 0.002336973833157695180, 0.004673709593152015201 ),
 .UNSPECIFIED. ) ;
#2495 = CARTESIAN_POINT ( 'NONE',  ( 5.000000000000004441, -2.342598717236951789, 4.057500000000047180 ) ) ;
#2496 = ADVANCED_FACE ( 'NONE', ( #3546 ), #6256, .F. ) ;
#2497 = AXIS2_PLACEMENT_3D ( 'NONE', #5703, #4371, #5556 ) ;
#2498 = AXIS2_PLACEMENT_3D ( 'NONE', #3469, #6790, #6914 ) ;
#2499 = VERTEX_POINT ( 'NONE', #4932 ) ;
#2500 = AXIS2_PLACEMENT_3D ( 'NONE', #848, #6172, #7420 ) ;
#2501 = LINE ( 'NONE', #5151, #2267 ) ;
#2502 = EDGE_LOOP ( 'NONE', ( #3415, #555, #4557, #3705, #4800, #2435 ) ) ;
#2503 = CARTESIAN_POINT ( 'NONE',  ( -8.000000000000007105, -4.618802153517398423, -7.685468820183672278 ) ) ;
#2504 = PRESENTATION_LAYER_ASSIGNMENT (  '', '', ( #8211 ) ) ;
#2505 = MECHANICAL_DESIGN_GEOMETRIC_PRESENTATION_REPRESENTATION (  '', ( #3893 ), #6833 ) ;
#2506 = DIRECTION ( 'NONE',  ( -1.000000000000000000, -8.881784197001244435E-16, 0.000000000000000000 ) ) ;
#2507 = DIRECTION ( 'NONE',  ( 0.000000000000000000, -1.024214141749972931E-29, 1.000000000000000000 ) ) ;
#2508 = DIRECTION ( 'NONE',  ( 0.000000000000000000, 0.000000000000000000, -1.000000000000000000 ) ) ;
#2509 = LINE ( 'NONE', #4553, #1832 ) ;
#2510 = COLOUR_RGB ( '',0.7921568627450980005, 0.8196078431372548767, 0.9333333333333333481 ) ;
#2511 = DIRECTION ( 'NONE',  ( 1.000000000000000000, 0.000000000000000000, 0.000000000000000000 ) ) ;
#2512 = PLANE ( 'NONE',  #1881 ) ;
#2513 = ADVANCED_FACE ( 'NONE', ( #8122 ), #1453, .T. ) ;
#2514 = DIRECTION ( 'NONE',  ( -3.851859888774471706E-33, -1.232595164407830946E-32, -1.000000000000000000 ) ) ;
#2515 = VERTEX_POINT ( 'NONE', #5514 ) ;
#2516 = CARTESIAN_POINT ( 'NONE',  ( -79.99999999999972999, 15.00000000000012434, 1.942890293094023946E-13 ) ) ;
#2517 = EDGE_CURVE ( 'NONE', #896, #4276, #7229, .T. ) ;
#2518 = DIRECTION ( 'NONE',  ( 0.000000000000000000, 1.000000000000000000, 0.000000000000000000 ) ) ;
#2519 = ADVANCED_FACE ( 'NONE', ( #2804 ), #3500, .T. ) ;
#2520 = DIRECTION ( 'NONE',  ( 0.000000000000000000, 0.000000000000000000, -1.000000000000000000 ) ) ;
#2521 = ORIENTED_EDGE ( 'NONE', *, *, #592, .F. ) ;
#2522 = DIRECTION ( 'NONE',  ( 1.000000000000000000, 0.000000000000000000, 0.000000000000000000 ) ) ;
#2523 = ORIENTED_EDGE ( 'NONE', *, *, #6074, .T. ) ;
#2524 = CARTESIAN_POINT ( 'NONE',  ( 0.000000000000000000, -3.469446951953614189E-15, 130.0000000000000000 ) ) ;
#2525 = ORIENTED_EDGE ( 'NONE', *, *, #7464, .T. ) ;
#2526 = PLANE ( 'NONE',  #4830 ) ;
#2527 = EDGE_CURVE ( 'NONE', #4401, #6993, #973, .T. ) ;
#2528 = DIRECTION ( 'NONE',  ( -1.000000000000000000, 3.549874073494553124E-30, 3.778304382545602261E-59 ) ) ;
#2529 = VECTOR ( 'NONE', #4259, 1000.000000000000000 ) ;
#2530 = B_SPLINE_CURVE_WITH_KNOTS ( 'NONE', 3,
 ( #5765, #8397, #3165, #2426, #1898, #1854, #7733, #5077 ),
 .UNSPECIFIED., .F., .F.,
 ( 4, 2, 2, 4 ),
 ( 0.004673709593152105407, 0.005837709341827624319, 0.007001709090503143232, 0.009329708587854177587 ),
 .UNSPECIFIED. ) ;
#2531 = CARTESIAN_POINT ( 'NONE',  ( 7.999999999999340972, -4.618802153516732290, -8.400000000000018119 ) ) ;
#2532 = EDGE_LOOP ( 'NONE', ( #996, #1240, #8282 ) ) ;
#2533 = CIRCLE ( 'NONE', #1427, 10.49999999999999645 ) ;
#2534 = DIRECTION ( 'NONE',  ( 0.000000000000000000, 0.000000000000000000, 1.000000000000000000 ) ) ;
#2535 = AXIS2_PLACEMENT_3D ( 'NONE', #5424, #6641, #7425 ) ;
#2536 = SHAPE_REPRESENTATION ( 'Conveyor roller', ( #7563 ), #1996 ) ;
#2537 = EDGE_CURVE ( 'NONE', #4358, #7854, #5861, .T. ) ;
#2538 = AXIS2_PLACEMENT_3D ( 'NONE', #4621, #742, #1960 ) ;
#2539 = DIRECTION ( 'NONE',  ( 0.000000000000000000, 0.000000000000000000, 1.000000000000000000 ) ) ;
#2540 = ORIENTED_EDGE ( 'NONE', *, *, #6020, .T. ) ;
#2541 = LINE ( 'NONE', #1932, #844 ) ;
#2542 = VECTOR ( 'NONE', #4532, 1000.000000000000000 ) ;
#2543 = EDGE_LOOP ( 'NONE', ( #712, #1727, #7595, #7600, #4582, #2031 ) ) ;
#2544 = AXIS2_PLACEMENT_3D ( 'NONE', #8108, #3446, #2148 ) ;
#2545 = CARTESIAN_POINT ( 'NONE',  ( 3.318518101602916381, 7.321656987762904301, 1.790627650495590601E-14 ) ) ;
#2546 = EDGE_LOOP ( 'NONE', ( #6536, #1351, #563, #5959 ) ) ;
#2547 = PRODUCT_DEFINITION_CONTEXT ( 'detailed design', #120, 'design' ) ;
#2548 = EDGE_CURVE ( 'NONE', #6113, #113, #2089, .T. ) ;
#2549 = FACE_BOUND ( 'NONE', #6675, .T. ) ;
#2550 = CARTESIAN_POINT ( 'NONE',  ( 9.184850993605156622E-15, -299.9999999999999432, -75.00000000000008527 ) ) ;
#2551 = FACE_OUTER_BOUND ( 'NONE', #4187, .T. ) ;
#2552 = CARTESIAN_POINT ( 'NONE',  ( 0.000000000000000000, 0.000000000000000000, 0.000000000000000000 ) ) ;
#2553 = VECTOR ( 'NONE', #573, 1000.000000000000000 ) ;
#2554 = DIRECTION ( 'NONE',  ( 0.000000000000000000, 1.000000000000000000, 1.795949010423047374E-16 ) ) ;
#2555 = AXIS2_PLACEMENT_3D ( 'NONE', #4993, #389, #3036 ) ;
#2556 = CARTESIAN_POINT ( 'NONE',  ( 8.000000000000015987, -3.867591403078991519, -7.902324684675471111 ) ) ;
#2557 = ORIENTED_EDGE ( 'NONE', *, *, #7048, .F. ) ;
#2558 =( NAMED_UNIT ( * ) SI_UNIT ( $, .STERADIAN. ) SOLID_ANGLE_UNIT ( ) );
#2559 = VERTEX_POINT ( 'NONE', #6991 ) ;
#2560 = FACE_OUTER_BOUND ( 'NONE', #2493, .T. ) ;
#2561 = EDGE_CURVE ( 'NONE', #3046, #1504, #1519, .T. ) ;
#2562 = CARTESIAN_POINT ( 'NONE',  ( 4.000000000000003553, -6.928203230275542523, 0.000000000000000000 ) ) ;
#2563 = CARTESIAN_POINT ( 'NONE',  ( 8.000000000000007105, 0.000000000000000000, -8.400000000000018119 ) ) ;
#2564 = ORIENTED_EDGE ( 'NONE', *, *, #7429, .F. ) ;
#2565 = CARTESIAN_POINT ( 'NONE',  ( 4.000000000000003553, 6.928203230275431501, -8.400000000000018119 ) ) ;
#2566 = ORIENTED_EDGE ( 'NONE', *, *, #3303, .F. ) ;
#2567 = MECHANICAL_DESIGN_GEOMETRIC_PRESENTATION_REPRESENTATION (  '', ( #5303 ), #6009 ) ;
#2568 = EDGE_LOOP ( 'NONE', ( #1108, #2582, #5161, #5593 ) ) ;
#2569 = AXIS2_PLACEMENT_3D ( 'NONE', #7310, #5401, #8011 ) ;
#2570 = EDGE_CURVE ( 'NONE', #5906, #7803, #5731, .T. ) ;
#2571 = CARTESIAN_POINT ( 'NONE',  ( -1.313474075707240729, -8.479269695850863542, -8.083279549040174317 ) ) ;
#2572 = ORIENTED_EDGE ( 'NONE', *, *, #7492, .F. ) ;
#2573 = CARTESIAN_POINT ( 'NONE',  ( 10.00000000000001599, 6.613092715395470808E-16, 5.400000000000479083 ) ) ;
#2574 = FACE_BOUND ( 'NONE', #2062, .T. ) ;
#2575 = CARTESIAN_POINT ( 'NONE',  ( 0.000000000000000000, 0.000000000000000000, 0.000000000000000000 ) ) ;
#2576 = CARTESIAN_POINT ( 'NONE',  ( -15.00000000000000000, -1.107409611084418900E-31, 18.00000000000000355 ) ) ;
#2577 = ORIENTED_EDGE ( 'NONE', *, *, #1227, .F. ) ;
#2578 = CARTESIAN_POINT ( 'NONE',  ( -6.661338147750939243E-13, -9.237604307034352757, -7.685468820183672278 ) ) ;
#2579 = AXIS2_PLACEMENT_3D ( 'NONE', #1897, #6474, #7999 ) ;
#2580 = PRODUCT_CONTEXT ( 'NONE', #2345, 'mechanical' ) ;
#2581 = AXIS2_PLACEMENT_3D ( 'NONE', #4258, #3607, #1473 ) ;
#2582 = ORIENTED_EDGE ( 'NONE', *, *, #7597, .T. ) ;
#2583 = CARTESIAN_POINT ( 'NONE',  ( 1.313474075707348421, 8.479269695850897293, -0.3167204509598749440 ) ) ;
#2584 = LINE ( 'NONE', #6545, #1792 ) ;
#2585 = SHAPE_REPRESENTATION_RELATIONSHIP ( 'NONE' , 'NONE' ,  #3455, #4586 ) ;
#2586 = ORIENTED_EDGE ( 'NONE', *, *, #4901, .T. ) ;
#2587 = ADVANCED_FACE ( 'NONE', ( #1696 ), #840, .T. ) ;
#2588 = PLANE ( 'NONE',  #2687 ) ;
#2589 = ORIENTED_EDGE ( 'NONE', *, *, #2474, .F. ) ;
#2590 = LINE ( 'NONE', #1890, #6171 ) ;
#2591 = CARTESIAN_POINT ( 'NONE',  ( 0.000000000000000000, 0.000000000000000000, 0.000000000000000000 ) ) ;
#2592 = DIRECTION ( 'NONE',  ( -1.463706757734299248E-32, 1.000000000000000000, 5.238529448733281520E-32 ) ) ;
#2593 = DIRECTION ( 'NONE',  ( 1.885870601543981347E-30, -1.000000000000000000, 7.405124331421681105E-16 ) ) ;
#2594 = CARTESIAN_POINT ( 'NONE',  ( 0.000000000000000000, 0.000000000000000000, 0.000000000000000000 ) ) ;
#2595 = ORIENTED_EDGE ( 'NONE', *, *, #535, .F. ) ;
#2596 = ADVANCED_FACE ( 'NONE', ( #6383 ), #3880, .T. ) ;
#2597 = VERTEX_POINT ( 'NONE', #3720 ) ;
#2598 = DIRECTION ( 'NONE',  ( 0.000000000000000000, 0.000000000000000000, -1.000000000000000000 ) ) ;
#2599 = B_SPLINE_CURVE_WITH_KNOTS ( 'NONE', 3,
 ( #3677, #2445, #5983, #7717, #7632, #7758 ),
 .UNSPECIFIED., .F., .F.,
 ( 4, 2, 4 ),
 ( 2.380731633751448567E-07, 0.002336973833157695180, 0.004673709593152015201 ),
 .UNSPECIFIED. ) ;
#2600 = PLANE ( 'NONE',  #4361 ) ;
#2601 = CARTESIAN_POINT ( 'NONE',  ( 8.000000000000229150, 3.871967595402074913, -0.4989386132325618339 ) ) ;
#2602 = CARTESIAN_POINT ( 'NONE',  ( -4.681481898396988583, 6.534749472788051960, 5.236696493104986416E-14 ) ) ;
#2603 = VERTEX_POINT ( 'NONE', #651 ) ;
#2604 = DIRECTION ( 'NONE',  ( -1.000000000000000000, -8.881784197001244435E-16, 0.000000000000000000 ) ) ;
#2605 = ORIENTED_EDGE ( 'NONE', *, *, #4352, .T. ) ;
#2606 = B_SPLINE_CURVE_WITH_KNOTS ( 'NONE', 3,
 ( #1728, #553, #7826, #5081, #1165, #5852 ),
 .UNSPECIFIED., .F., .F.,
 ( 4, 2, 4 ),
 ( 2.380731630324309322E-07, 0.002336973833157509998, 0.004673709593151987446 ),
 .UNSPECIFIED. ) ;
#2607 = EDGE_CURVE ( 'NONE', #2608, #2801, #2599, .T. ) ;
#2608 = VERTEX_POINT ( 'NONE', #6342 ) ;
#2609 = LINE ( 'NONE', #699, #1013 ) ;
#2610 = EDGE_LOOP ( 'NONE', ( #8303, #1573, #2915, #792 ) ) ;
#2611 = CARTESIAN_POINT ( 'NONE',  ( 0.000000000000000000, 60.00000000000000000, -50.00000000000000000 ) ) ;
#2612 = DIRECTION ( 'NONE',  ( 1.000000000000000000, 0.000000000000000000, 0.000000000000000000 ) ) ;
#2613 = CARTESIAN_POINT ( 'NONE',  ( 10.00000000000000888, -650.0000000000002274, 79.99999999999995737 ) ) ;
#2614 = CIRCLE ( 'NONE', #8587, 25.00000000000000711 ) ;
#2615 = DIRECTION ( 'NONE',  ( -1.000000000000000000, 1.774937036747276562E-30, 0.000000000000000000 ) ) ;
#2616 = CARTESIAN_POINT ( 'NONE',  ( -50.00000000000004263, -425.0000000000000000, 3.469446951953614189E-15 ) ) ;
#2617 = ORIENTED_EDGE ( 'NONE', *, *, #3255, .F. ) ;
#2618 = EDGE_CURVE ( 'NONE', #6546, #3749, #4158, .T. ) ;
#2619 = EDGE_CURVE ( 'NONE', #4829, #2216, #7799, .T. ) ;
#2620 = PRODUCT_RELATED_PRODUCT_CATEGORY ( 'part', '', ( #6615 ) ) ;
#2621 = APPLICATION_PROTOCOL_DEFINITION ( 'draft international standard', 'automotive_design', 1998, #4138 ) ;
#2622 = ADVANCED_BREP_SHAPE_REPRESENTATION ( '', ( #132, #7563 ), #3529 ) ;
#2623 = EDGE_CURVE ( 'NONE', #6630, #4756, #8454, .T. ) ;
#2624 = CARTESIAN_POINT ( 'NONE',  ( 5.499999999999999112, 60.00000000000000000, -45.00000000000000711 ) ) ;
#2625 = ORIENTED_EDGE ( 'NONE', *, *, #4808, .F. ) ;
#2626 = AXIS2_PLACEMENT_3D ( 'NONE', #4703, #6109, #7845 ) ;
#2627 = CARTESIAN_POINT ( 'NONE',  ( 4.000000000000003553, 9.714451465470119729E-14, 0.000000000000000000 ) ) ;
#2628 = CONICAL_SURFACE ( 'NONE', #830, 24.49999999999999645, 0.7853981633974503884 ) ;
#2629 = DIRECTION ( 'NONE',  ( -2.266822170910512774E-17, 0.9627900128470828767, -0.2702506080694626611 ) ) ;
#2630 = VERTEX_POINT ( 'NONE', #4411 ) ;
#2631 = CYLINDRICAL_SURFACE ( 'NONE', #4351, 10.50000000000001066 ) ;
#2632 = ORIENTED_EDGE ( 'NONE', *, *, #4023, .F. ) ;
#2633 = CARTESIAN_POINT ( 'NONE',  ( 5.500000000000000000, 0.000000000000000000, 50.00000000000000000 ) ) ;
#2634 =( REPRESENTATION_RELATIONSHIP ('NONE','NONE', #1279, #6122 ) REPRESENTATION_RELATIONSHIP_WITH_TRANSFORMATION ( #7933 )SHAPE_REPRESENTATION_RELATIONSHIP( ) );
#2635 = AXIS2_PLACEMENT_3D ( 'NONE', #1424, #770, #4650 ) ;
#2636 = DIRECTION ( 'NONE',  ( 1.000000000000000000, -1.774937036747276562E-30, 0.000000000000000000 ) ) ;
#2637 = DIRECTION ( 'NONE',  ( -2.728201748236299157E-33, 0.7071067811865321406, -0.7071067811865628938 ) ) ;
#2638 = LINE ( 'NONE', #4079, #3473 ) ;
#2639 = CARTESIAN_POINT ( 'NONE',  ( -49.99999999999954525, 120.0000000000003268, 0.000000000000000000 ) ) ;
#2640 = DIRECTION ( 'NONE',  ( -0.000000000000000000, -0.000000000000000000, 1.000000000000000000 ) ) ;
#2641 = VERTEX_POINT ( 'NONE', #6458 ) ;
#2642 = AXIS2_PLACEMENT_3D ( 'NONE', #5419, #3545, #4844 ) ;
#2643 = DIRECTION ( 'NONE',  ( 3.821045009664296251E-30, -3.944304526105037307E-30, 1.000000000000000000 ) ) ;
#2644 = CARTESIAN_POINT ( 'NONE',  ( 1.000000000000000888, 9.797174393176622763E-16, -8.000000000000001776 ) ) ;
#2645 = CARTESIAN_POINT ( 'NONE',  ( 50.00000000000004263, -500.0000000000000000, 50.00000000000000000 ) ) ;
#2646 = CLOSED_SHELL ( 'NONE', ( #5216, #5927, #8119, #197, #6352, #3334, #1532, #8317, #7724, #4958, #6191, #1545, #6666, #8096, #6498, #5080, #6288, #1833, #5942, #5098, #673, #753 ) ) ;
#2647 = PRESENTATION_LAYER_ASSIGNMENT (  '', '', ( #2791 ) ) ;
#2648 = LINE ( 'NONE', #11, #4540 ) ;
#2649 = CARTESIAN_POINT ( 'NONE',  ( -4.339467034331305761, -6.732211846623399332, -8.399999999999982592 ) ) ;
#2650 = MECHANICAL_DESIGN_GEOMETRIC_PRESENTATION_REPRESENTATION (  '', ( #3897 ), #7523 ) ;
#2651 = CARTESIAN_POINT ( 'NONE',  ( 4.000000000000003553, 6.928203230275597591, -8.400000000000018119 ) ) ;
#2652 = CARTESIAN_POINT ( 'NONE',  ( -7.999999999999888978, 0.7809653281574864270, -8.400000000000089173 ) ) ;
#2653 = EDGE_CURVE ( 'NONE', #7133, #2971, #7113, .T. ) ;
#2654 = CARTESIAN_POINT ( 'NONE',  ( -2.220446049250313081E-13, -650.0000000000000000, 79.99999999999995737 ) ) ;
#2655 = CYLINDRICAL_SURFACE ( 'NONE', #57, 5.500000000000024869 ) ;
#2656 = EDGE_LOOP ( 'NONE', ( #7625, #5641 ) ) ;
#2657 = CONICAL_SURFACE ( 'NONE', #2363, 8.000000000000007105, 1.047197551196597631 ) ;
#2658 = DIRECTION ( 'NONE',  ( 0.000000000000000000, -5.908893405598423146E-30, 1.000000000000000000 ) ) ;
#2659 = EDGE_LOOP ( 'NONE', ( #8344, #7426 ) ) ;
#2660 = LINE ( 'NONE', #7836, #7682 ) ;
#2661 = ORIENTED_EDGE ( 'NONE', *, *, #3116, .F. ) ;
#2662 = LINE ( 'NONE', #5316, #7018 ) ;
#2663 = EDGE_CURVE ( 'NONE', #2214, #4846, #2922, .T. ) ;
#2664 = CARTESIAN_POINT ( 'NONE',  ( -4.680456609904129373, -6.535341423375579772, -8.383111142572207797 ) ) ;
#2665 = AXIS2_PLACEMENT_3D ( 'NONE', #3637, #7028, #3719 ) ;
#2666 = CARTESIAN_POINT ( 'NONE',  ( 2.220446049250313081E-13, 9.237604307034075646, -7.685468820183672278 ) ) ;
#2667 = EDGE_CURVE ( 'NONE', #6993, #8513, #5190, .T. ) ;
#2668 = DIRECTION ( 'NONE',  ( 0.000000000000000000, 0.000000000000000000, 1.000000000000000000 ) ) ;
#2669 = ORIENTED_EDGE ( 'NONE', *, *, #6166, .F. ) ;
#2670 = SHAPE_DEFINITION_REPRESENTATION ( #4043, #4603 ) ;
#2671 = DIRECTION ( 'NONE',  ( -1.000000000000000000, 1.284024588418159550E-35, 0.000000000000000000 ) ) ;
#2672 = EDGE_CURVE ( 'NONE', #3749, #8505, #3063, .T. ) ;
#2673 = ORIENTED_EDGE ( 'NONE', *, *, #7484, .F. ) ;
#2674 = CARTESIAN_POINT ( 'NONE',  ( 1.630253220555408214E-45, 9.184850993604743653E-16, 7.000000000000000888 ) ) ;
#2675 = FACE_OUTER_BOUND ( 'NONE', #608, .T. ) ;
#2676 = ORIENTED_EDGE ( 'NONE', *, *, #6819, .T. ) ;
#2677 = AXIS2_PLACEMENT_3D ( 'NONE', #4713, #7529, #8177 ) ;
#2678 = EDGE_CURVE ( 'NONE', #8055, #5227, #4869, .T. ) ;
#2679 = DIRECTION ( 'NONE',  ( 0.000000000000000000, 1.000000000000000000, 0.000000000000000000 ) ) ;
#2680 = ORIENTED_EDGE ( 'NONE', *, *, #6981, .F. ) ;
#2681 = DIRECTION ( 'NONE',  ( 0.000000000000000000, -5.322451846059955323E-30, 1.000000000000000000 ) ) ;
#2682 = AXIS2_PLACEMENT_3D ( 'NONE', #6317, #4985, #8431 ) ;
#2683 = EDGE_CURVE ( 'NONE', #1627, #7390, #2045, .T. ) ;
#2684 = FACE_BOUND ( 'NONE', #3726, .T. ) ;
#2685 = CARTESIAN_POINT ( 'NONE',  ( -8.000000000000227374, 3.115336682266928836, -0.3193931313916110737 ) ) ;
#2686 = AXIS2_PLACEMENT_3D ( 'NONE', #8023, #172, #5457 ) ;
#2687 = AXIS2_PLACEMENT_3D ( 'NONE', #7204, #6504, #537 ) ;
#2688 = CARTESIAN_POINT ( 'NONE',  ( 8.000000000000117240, 4.618802153517009401, -0.7145311798163467287 ) ) ;
#2689 = PLANE ( 'NONE',  #2579 ) ;
#2690 = CYLINDRICAL_SURFACE ( 'NONE', #189, 75.00000000000000000 ) ;
#2691 = ORIENTED_EDGE ( 'NONE', *, *, #2623, .T. ) ;
#2692 = CARTESIAN_POINT ( 'NONE',  ( 0.000000000000000000, 299.9999999999999432, 24.49999999999994316 ) ) ;
#2693 = SURFACE_STYLE_USAGE ( .BOTH. , #5394 ) ;
#2694 = DIRECTION ( 'NONE',  ( 0.000000000000000000, 0.000000000000000000, -1.000000000000000000 ) ) ;
#2695 = DIRECTION ( 'NONE',  ( 1.463706757734299248E-32, -1.000000000000000000, 4.930380657631321594E-32 ) ) ;
#2696 = LINE ( 'NONE', #5355, #6774 ) ;
#2697 = AXIS2_PLACEMENT_3D ( 'NONE', #2594, #1986, #4693 ) ;
#2698 = CARTESIAN_POINT ( 'NONE',  ( 4.000000000000003553, -6.928203230275542523, 0.000000000000000000 ) ) ;
#2699 = VECTOR ( 'NONE', #4353, 1000.000000000000114 ) ;
#2700 = CARTESIAN_POINT ( 'NONE',  ( -6.661338147750939243E-13, 9.237604307034352757, -7.685468820183672278 ) ) ;
#2701 = VERTEX_POINT ( 'NONE', #116 ) ;
#2702 = DIRECTION ( 'NONE',  ( 0.000000000000000000, 0.000000000000000000, -1.000000000000000000 ) ) ;
#2703 = VERTEX_POINT ( 'NONE', #2828 ) ;
#2704 = EDGE_CURVE ( 'NONE', #1716, #303, #6156, .T. ) ;
#2705 =( GEOMETRIC_REPRESENTATION_CONTEXT ( 3 ) GLOBAL_UNCERTAINTY_ASSIGNED_CONTEXT ( ( #105 ) ) GLOBAL_UNIT_ASSIGNED_CONTEXT ( ( #1753, #6390, #5067 ) ) REPRESENTATION_CONTEXT ( 'NONE', 'WORKASPACE' ) );
#2706 = CARTESIAN_POINT ( 'NONE',  ( 0.000000000000000000, -9.237604307034018802, -7.685468820183672278 ) ) ;
#2707 = ORIENTED_EDGE ( 'NONE', *, *, #6829, .T. ) ;
#2708 = LINE ( 'NONE', #7274, #6315 ) ;
#2709 = CARTESIAN_POINT ( 'NONE',  ( -8.000000000000007105, 0.000000000000000000, -8.400000000000018119 ) ) ;
#2710 = CARTESIAN_POINT ( 'NONE',  ( 50.00000000000004263, 425.0000000000000000, -3.469446951953614189E-15 ) ) ;
#2711 = CARTESIAN_POINT ( 'NONE',  ( -31.74999999999994316, -4.257395394114594689E-29, 4.000000000000030198 ) ) ;
#2712 = ORIENTED_EDGE ( 'NONE', *, *, #5928, .T. ) ;
#2713 = PRODUCT_CONTEXT ( 'NONE', #7696, 'mechanical' ) ;
#2714 = PLANE ( 'NONE',  #1980 ) ;
#2715 = ORIENTED_EDGE ( 'NONE', *, *, #2809, .T. ) ;
#2716 = CONTEXT_DEPENDENT_SHAPE_REPRESENTATION ( #862, #63 ) ;
#2717 = EDGE_CURVE ( 'NONE', #5352, #3689, #6025, .T. ) ;
#2718 = FILL_AREA_STYLE_COLOUR ( '', #3442 ) ;
#2719 = CARTESIAN_POINT ( 'NONE',  ( 275.0000000000000000, -425.0000000000000000, 75.00000000000000000 ) ) ;
#2720 = ORIENTED_EDGE ( 'NONE', *, *, #4512, .T. ) ;
#2721 = AXIS2_PLACEMENT_3D ( 'NONE', #3006, #1056, #8321 ) ;
#2722 = CARTESIAN_POINT ( 'NONE',  ( -45.49999999999963762, 87.50000000000036948, 9.999999999999786837 ) ) ;
#2723 = CARTESIAN_POINT ( 'NONE',  ( 0.000000000000000000, 299.9999999999999432, -6.938893903907228378E-14 ) ) ;
#2724 = ORIENTED_EDGE ( 'NONE', *, *, #8104, .T. ) ;
#2725 = ADVANCED_FACE ( 'NONE', ( #2000, #3349 ), #19, .F. ) ;
#2726 = CONICAL_SURFACE ( 'NONE', #3269, 19.49999999999996803, 0.7853981633974507215 ) ;
#2727 = CARTESIAN_POINT ( 'NONE',  ( 5.080504117408896292, 2.106769544347820933, -8.400999999999992696 ) ) ;
#2728 = PRODUCT ( 'Rectangular section tube 100x100x5', 'Rectangular section tube 100x100x5', '', ( #3877 ) ) ;
#2729 = ORIENTED_EDGE ( 'NONE', *, *, #2619, .F. ) ;
#2730 = CARTESIAN_POINT ( 'NONE',  ( -5.500000000000000000, 6.735557395310442023E-16, 45.00000000000000000 ) ) ;
#2731 = FACE_OUTER_BOUND ( 'NONE', #8566, .T. ) ;
#2732 = DIRECTION ( 'NONE',  ( -3.851859888774471706E-33, -1.232595164407830946E-32, -1.000000000000000000 ) ) ;
#2733 = EDGE_CURVE ( 'NONE', #2515, #650, #1762, .T. ) ;
#2734 = CARTESIAN_POINT ( 'NONE',  ( 32.49999999999997158, 1.387778780781445676E-14, 0.000000000000000000 ) ) ;
#2735 = CARTESIAN_POINT ( 'NONE',  ( -3.660532965668796823, 7.124194613927540054, 5.481721948921974147E-14 ) ) ;
#2736 = CARTESIAN_POINT ( 'NONE',  ( 6.689127551062064470, 5.375634714784610857, -0.3173508448886774302 ) ) ;
#2737 = EDGE_LOOP ( 'NONE', ( #8037, #4902, #6393 ) ) ;
#2738 = PRESENTATION_STYLE_ASSIGNMENT (( #685 ) ) ;
#2739 = FILL_AREA_STYLE_COLOUR ( '', #6283 ) ;
#2740 = AXIS2_PLACEMENT_3D ( 'NONE', #3295, #5307, #4041 ) ;
#2741 = CARTESIAN_POINT ( 'NONE',  ( -8.000000000000007105, 4.618802153517009401, -0.7145311798163467287 ) ) ;
#2742 = LINE ( 'NONE', #6704, #4720 ) ;
#2743 = AXIS2_PLACEMENT_3D ( 'NONE', #7812, #1849, #5030 ) ;
#2744 = LINE ( 'NONE', #782, #7445 ) ;
#2745 = ORIENTED_EDGE ( 'NONE', *, *, #7556, .T. ) ;
#2746 =( NAMED_UNIT ( * ) SI_UNIT ( $, .STERADIAN. ) SOLID_ANGLE_UNIT ( ) );
#2747 = ORIENTED_EDGE ( 'NONE', *, *, #1847, .T. ) ;
#2748 = CARTESIAN_POINT ( 'NONE',  ( 10.40000000000001990, 0.000000000000000000, 4.440892098500626162E-13 ) ) ;
#2749 = FACE_OUTER_BOUND ( 'NONE', #3005, .T. ) ;
#2750 = CARTESIAN_POINT ( 'NONE',  ( -8.000000000000225597, -0.7805016046291537446, -8.399999999999890221 ) ) ;
#2751 = CARTESIAN_POINT ( 'NONE',  ( 0.000000000000000000, 0.000000000000000000, -8.400000000000018119 ) ) ;
#2752 = CARTESIAN_POINT ( 'NONE',  ( -8.000000000000003553, -0.7805016046290103038, -8.400000000000023448 ) ) ;
#2753 = PRODUCT_DEFINITION ( 'UNKNOWN', '', #8136, #5248 ) ;
#2754 = ORIENTED_EDGE ( 'NONE', *, *, #3471, .F. ) ;
#2755 = ORIENTED_EDGE ( 'NONE', *, *, #6644, .T. ) ;
#2756 = EDGE_CURVE ( 'NONE', #7472, #6028, #1529, .T. ) ;
#2757 = EDGE_LOOP ( 'NONE', ( #175, #5288, #7117, #377 ) ) ;
#2758 = CARTESIAN_POINT ( 'NONE',  ( -19.99999999999986855, 15.00000000000012434, 0.000000000000000000 ) ) ;
#2759 = AXIS2_PLACEMENT_3D ( 'NONE', #6982, #3002, #8237 ) ;
#2760 = ORIENTED_EDGE ( 'NONE', *, *, #1100, .F. ) ;
#2761 = CARTESIAN_POINT ( 'NONE',  ( 0.000000000000000000, -3.469446951953614189E-15, 130.0000000000000000 ) ) ;
#2762 = VERTEX_POINT ( 'NONE', #8101 ) ;
#2763 = DIRECTION ( 'NONE',  ( 1.000000000000000000, 8.881784197001244435E-16, 0.000000000000000000 ) ) ;
#2764 = ADVANCED_FACE ( 'NONE', ( #4093 ), #7655, .T. ) ;
#2765 = B_SPLINE_CURVE_WITH_KNOTS ( 'NONE', 3,
 ( #6593, #1224, #6684, #713, #8585, #8032 ),
 .UNSPECIFIED., .F., .F.,
 ( 4, 2, 4 ),
 ( 0.01291313371729461458, 0.01525081363757315941, 0.01758849355785170598 ),
 .UNSPECIFIED. ) ;
#2766 = LINE ( 'NONE', #8128, #6235 ) ;
#2767 = EDGE_CURVE ( 'NONE', #4141, #4545, #4463, .T. ) ;
#2768 = EDGE_LOOP ( 'NONE', ( #8360, #2617, #1966, #3991 ) ) ;
#2769 = CARTESIAN_POINT ( 'NONE',  ( -0.6527133886637689342, 8.860760056386036254, -0.4969600502619508364 ) ) ;
#2770 = CARTESIAN_POINT ( 'NONE',  ( 0.000000000000000000, -3.469446951953614189E-15, 130.0000000000000000 ) ) ;
#2771 = CARTESIAN_POINT ( 'NONE',  ( -275.0000000000000000, -425.0000000000000000, -80.00000000000000000 ) ) ;
#2772 = CARTESIAN_POINT ( 'NONE',  ( -5.355005115541064953, -6.145890662064632082, -0.08224679563976682040 ) ) ;
#2773 = ORIENTED_EDGE ( 'NONE', *, *, #3587, .T. ) ;
#2774 = CARTESIAN_POINT ( 'NONE',  ( 6.689127551062092003, 5.375634714784659707, -0.3173508448887064071 ) ) ;
#2775 = ORIENTED_EDGE ( 'NONE', *, *, #5681, .T. ) ;
#2776 = MANIFOLD_SOLID_BREP ( 'Base-Revolve', #1243 ) ;
#2777 = DIRECTION ( 'NONE',  ( -1.000000000000000000, 0.000000000000000000, 0.000000000000000000 ) ) ;
#2778 = CARTESIAN_POINT ( 'NONE',  ( -6.686525924292721079, 5.377136764700112259, -0.3167204509597890683 ) ) ;
#2779 = EDGE_CURVE ( 'NONE', #1989, #5906, #5006, .T. ) ;
#2780 = VECTOR ( 'NONE', #3799, 1000.000000000000000 ) ;
#2781 = CARTESIAN_POINT ( 'NONE',  ( 5.551115123125782702E-14, 3.518949890710790118, 2.220446049250313081E-13 ) ) ;
#2782 = DIRECTION ( 'NONE',  ( -0.9237280213470678847, -0.3830490080632384942, 0.000000000000000000 ) ) ;
#2783 = ORIENTED_EDGE ( 'NONE', *, *, #2793, .F. ) ;
#2784 = DIRECTION ( 'NONE',  ( 6.400024471206996205E-36, -1.000000000000000000, 0.000000000000000000 ) ) ;
#2785 = ORIENTED_EDGE ( 'NONE', *, *, #8184, .T. ) ;
#2786 = CARTESIAN_POINT ( 'NONE',  ( -2.645508037661986389, -7.710219529346967526, -0.06809871960565012927 ) ) ;
#2787 = DIRECTION ( 'NONE',  ( 0.000000000000000000, -0.000000000000000000, 1.000000000000000000 ) ) ;
#2788 =( GEOMETRIC_REPRESENTATION_CONTEXT ( 3 ) GLOBAL_UNCERTAINTY_ASSIGNED_CONTEXT ( ( #7959 ) ) GLOBAL_UNIT_ASSIGNED_CONTEXT ( ( #7490, #6708, #2746 ) ) REPRESENTATION_CONTEXT ( 'NONE', 'WORKASPACE' ) );
#2789 = EDGE_CURVE ( 'NONE', #5471, #3289, #7370, .T. ) ;
#2790 = CARTESIAN_POINT ( 'NONE',  ( 0.000000000000000000, -3.518949890710769690, 0.000000000000000000 ) ) ;
#2791=STYLED_ITEM('',(#8670),#5753);
#2792 = EDGE_LOOP ( 'NONE', ( #2557, #7809, #2898, #4770 ) ) ;
#2793 = EDGE_CURVE ( 'NONE', #1712, #3620, #432, .T. ) ;
#2794 = DIRECTION ( 'NONE',  ( 1.000000000000000000, 0.000000000000000000, -0.000000000000000000 ) ) ;
#2795 = ORIENTED_EDGE ( 'NONE', *, *, #5848, .F. ) ;
#2796 = ORIENTED_EDGE ( 'NONE', *, *, #2548, .F. ) ;
#2797 = AXIS2_PLACEMENT_3D ( 'NONE', #8275, #3038, #2380 ) ;
#2798 = PRODUCT_DEFINITION_SHAPE ( 'NONE', 'NONE',  #8605 ) ;
#2799 = CARTESIAN_POINT ( 'NONE',  ( 0.000000000000000000, 0.000000000000000000, 18.00000000000000355 ) ) ;
#2800 = CARTESIAN_POINT ( 'NONE',  ( 10.40000000000001990, 2.874123996872394147E-29, -5.399999999999590905 ) ) ;
#2801 = VERTEX_POINT ( 'NONE', #3704 ) ;
#2802 = APPLICATION_CONTEXT ( 'automotive_design' ) ;
#2803 = DIRECTION ( 'NONE',  ( -3.919652622816902408E-30, -3.944304526105059027E-30, 1.000000000000000000 ) ) ;
#2804 = FACE_OUTER_BOUND ( 'NONE', #6816, .T. ) ;
#2805 = DIRECTION ( 'NONE',  ( -1.054711873393898713E-15, -0.9999999999999996669, 5.898059818321142888E-17 ) ) ;
#2806 = ORIENTED_EDGE ( 'NONE', *, *, #4919, .F. ) ;
#2807 = ORIENTED_EDGE ( 'NONE', *, *, #2161, .F. ) ;
#2808 = DIRECTION ( 'NONE',  ( 0.000000000000000000, 0.000000000000000000, -1.000000000000000000 ) ) ;
#2809 = EDGE_CURVE ( 'NONE', #5902, #7519, #7584, .T. ) ;
#2810 = CYLINDRICAL_SURFACE ( 'NONE', #1701, 5.500000000000023981 ) ;
#2811 = DIRECTION ( 'NONE',  ( -1.000000000000000000, -8.881784197001244435E-16, 0.000000000000000000 ) ) ;
#2812 = ORIENTED_EDGE ( 'NONE', *, *, #2779, .T. ) ;
#2813 = CARTESIAN_POINT ( 'NONE',  ( 8.000000000000007105, 2.775557561562884725E-14, 6.500000000000667022 ) ) ;
#2814 = CARTESIAN_POINT ( 'NONE',  ( 0.000000000000000000, 0.000000000000000000, 0.000000000000000000 ) ) ;
#2815 = FACE_OUTER_BOUND ( 'NONE', #5584, .T. ) ;
#2816 = VERTEX_POINT ( 'NONE', #7015 ) ;
#2817 = CARTESIAN_POINT ( 'NONE',  ( -7.999999999999896083, 4.618802153516899267, -0.7145311798163467287 ) ) ;
#2818 = CARTESIAN_POINT ( 'NONE',  ( -275.0000000000000000, 425.0000000000000000, -74.99999999999984368 ) ) ;
#2819 = AXIS2_PLACEMENT_3D ( 'NONE', #4626, #7237, #3919 ) ;
#2820 = EDGE_CURVE ( 'NONE', #7684, #5825, #278, .T. ) ;
#2821 = LINE ( 'NONE', #5486, #6047 ) ;
#2822 = AXIS2_PLACEMENT_3D ( 'NONE', #7111, #1136, #7154 ) ;
#2823 = B_SPLINE_CURVE_WITH_KNOTS ( 'NONE', 3,
 ( #2741, #1298, #6565, #8563, #2602, #645 ),
 .UNSPECIFIED., .F., .F.,
 ( 4, 2, 4 ),
 ( 2.380731628432377855E-07, 0.002336973833157452319, 0.004673709593152062039 ),
 .UNSPECIFIED. ) ;
#2824 = DIRECTION ( 'NONE',  ( -7.703719777548943412E-34, 0.000000000000000000, 1.000000000000000000 ) ) ;
#2825 = CARTESIAN_POINT ( 'NONE',  ( 0.000000000000000000, 0.000000000000000000, 0.000000000000000000 ) ) ;
#2826 = CARTESIAN_POINT ( 'NONE',  ( -4.000000000000891731, 6.928203230275542523, -8.400000000000018119 ) ) ;
#2827 = EDGE_LOOP ( 'NONE', ( #695, #6875, #6894, #4818 ) ) ;
#2828 = CARTESIAN_POINT ( 'NONE',  ( 39.75000000000000000, 4.867971026610730028E-15, 0.000000000000000000 ) ) ;
#2829 = EDGE_LOOP ( 'NONE', ( #3556, #7576 ) ) ;
#2830 = CIRCLE ( 'NONE', #1293, 6.500000000000002665 ) ;
#2831 = EDGE_CURVE ( 'NONE', #2603, #2349, #5871, .T. ) ;
#2832 = CARTESIAN_POINT ( 'NONE',  ( 0.000000000000000000, 0.000000000000000000, -8.400000000000018119 ) ) ;
#2833 = DIRECTION ( 'NONE',  ( 0.000000000000000000, 0.000000000000000000, 1.000000000000000000 ) ) ;
#2834 = CARTESIAN_POINT ( 'NONE',  ( 50.00000000000004263, 500.0000000000000000, 50.00000000000000000 ) ) ;
#2835 = ORIENTED_EDGE ( 'NONE', *, *, #4808, .T. ) ;
#2836 = CARTESIAN_POINT ( 'NONE',  ( -8.000000000000007105, -4.618802153517065356, -7.685468820183672278 ) ) ;
#2837 = EDGE_LOOP ( 'NONE', ( #1359, #5314, #2707, #5174 ) ) ;
#2838 = DIRECTION ( 'NONE',  ( 0.9237280213470678847, 0.3830490080632384942, 0.000000000000000000 ) ) ;
#2839 = EDGE_LOOP ( 'NONE', ( #6572, #7525, #6505, #4873 ) ) ;
#2840 = EDGE_CURVE ( 'NONE', #7133, #6524, #5682, .T. ) ;
#2841 = CIRCLE ( 'NONE', #3794, 4.400000000000030553 ) ;
#2842 = AXIS2_PLACEMENT_3D ( 'NONE', #3781, #2378, #7776 ) ;
#2843 = FACE_OUTER_BOUND ( 'NONE', #6654, .T. ) ;
#2844 = AXIS2_PLACEMENT_3D ( 'NONE', #5467, #1578, #2805 ) ;
#2845 = ORIENTED_EDGE ( 'NONE', *, *, #4946, .T. ) ;
#2846 = DIRECTION ( 'NONE',  ( 1.000000000000000000, 3.083952846180994816E-15, -3.821045009664285742E-30 ) ) ;
#2847 = DIRECTION ( 'NONE',  ( -1.058471975245258048E-16, 8.736544766236844851E-16, -1.000000000000000000 ) ) ;
#2848 = EDGE_LOOP ( 'NONE', ( #2881, #1447, #3011, #7362 ) ) ;
#2849 = PRODUCT_DEFINITION_FORMATION_WITH_SPECIFIED_SOURCE ( 'ANY', '', #552, .NOT_KNOWN. ) ;
#2850 = DIRECTION ( 'NONE',  ( 1.000000000000000000, 0.000000000000000000, -6.938893903907228378E-17 ) ) ;
#2851 = AXIS2_PLACEMENT_3D ( 'NONE', #1435, #694, #8099 ) ;
#2852 = ORIENTED_EDGE ( 'NONE', *, *, #6705, .T. ) ;
#2853 = DIRECTION ( 'NONE',  ( 0.000000000000000000, 1.000000000000000000, 0.000000000000000000 ) ) ;
#2854 = CIRCLE ( 'NONE', #7716, 8.000000000000007105 ) ;
#2855 = LINE ( 'NONE', #5521, #4020 ) ;
#2856 = VERTEX_POINT ( 'NONE', #6885 ) ;
#2857 = CARTESIAN_POINT ( 'NONE',  ( 4.339467034330982464, 6.732211846623266105, 1.328238011475783811E-13 ) ) ;
#2858 = EDGE_CURVE ( 'NONE', #5104, #3693, #1118, .T. ) ;
#2859 = CARTESIAN_POINT ( 'NONE',  ( 0.000000000000000000, 0.000000000000000000, 0.000000000000000000 ) ) ;
#2860 = EDGE_LOOP ( 'NONE', ( #7495, #6369, #7792, #8428 ) ) ;
#2861 = AXIS2_PLACEMENT_3D ( 'NONE', #1817, #7056, #1085 ) ;
#2862 = CARTESIAN_POINT ( 'NONE',  ( -4.680456609904036114, -6.535341423375559344, -0.01688885742777373675 ) ) ;
#2863 = DIRECTION ( 'NONE',  ( 3.733809166716685024E-60, -1.478898702612462838E-15, -1.000000000000000000 ) ) ;
#2864 = CARTESIAN_POINT ( 'NONE',  ( -14.24999999999984368, 15.00000000000014211, 10.00000000000000888 ) ) ;
#2865 = CARTESIAN_POINT ( 'NONE',  ( -49.99999999999944578, 152.5000000000003126, 9.999999999999786837 ) ) ;
#2866 = ADVANCED_FACE ( 'NONE', ( #2300, #4397 ), #1047, .T. ) ;
#2867 = DIRECTION ( 'NONE',  ( 3.919652622816902408E-30, 3.944304526105059027E-30, -1.000000000000000000 ) ) ;
#2868 = ORIENTED_EDGE ( 'NONE', *, *, #6386, .T. ) ;
#2869 = DIRECTION ( 'NONE',  ( 0.000000000000000000, 5.322451846059955323E-30, -1.000000000000000000 ) ) ;
#2870 = VERTEX_POINT ( 'NONE', #4263 ) ;
#2871 = CARTESIAN_POINT ( 'NONE',  ( -8.000000000000007105, 1.110223024625156540E-13, 0.000000000000000000 ) ) ;
#2872 = FACE_OUTER_BOUND ( 'NONE', #958, .T. ) ;
#2873 = DIRECTION ( 'NONE',  ( -1.000000000000000000, 1.774937036747276562E-30, 0.000000000000000000 ) ) ;
#2874 = ORIENTED_EDGE ( 'NONE', *, *, #5062, .T. ) ;
#2875 = ADVANCED_FACE ( 'NONE', ( #392 ), #5726, .T. ) ;
#2876 = ORIENTED_EDGE ( 'NONE', *, *, #6819, .F. ) ;
#2877 = AXIS2_PLACEMENT_3D ( 'NONE', #7868, #8603, #2694 ) ;
#2878 = CARTESIAN_POINT ( 'NONE',  ( 10.40000000000001990, 0.000000000000000000, 4.440892098500626162E-13 ) ) ;
#2879 = ADVANCED_FACE ( 'NONE', ( #5538 ), #1005, .T. ) ;
#2880 = DIRECTION ( 'NONE',  ( 0.000000000000000000, 0.000000000000000000, 1.000000000000000000 ) ) ;
#2881 = ORIENTED_EDGE ( 'NONE', *, *, #7184, .F. ) ;
#2882 = ADVANCED_FACE ( 'NONE', ( #4219 ), #5038, .T. ) ;
#2883 = CARTESIAN_POINT ( 'NONE',  ( -31.74999999999994316, 7.960204194458489674E-16, -6.500000000000001776 ) ) ;
#2884 = DIRECTION ( 'NONE',  ( 0.000000000000000000, -1.000000000000000000, -7.598173571352319403E-18 ) ) ;
#2885 = DIRECTION ( 'NONE',  ( 0.000000000000000000, 0.000000000000000000, -1.000000000000000000 ) ) ;
#2886 = ORIENTED_EDGE ( 'NONE', *, *, #5180, .F. ) ;
#2887 = DIRECTION ( 'NONE',  ( 6.400024471206997542E-36, -1.000000000000000000, 0.000000000000000000 ) ) ;
#2888 = ORIENTED_EDGE ( 'NONE', *, *, #3505, .T. ) ;
#2889 = CARTESIAN_POINT ( 'NONE',  ( 275.0000000000000000, -425.0000000000000000, 0.000000000000000000 ) ) ;
#2890 = EDGE_CURVE ( 'NONE', #6876, #3217, #2999, .T. ) ;
#2891 = B_SPLINE_CURVE_WITH_KNOTS ( 'NONE', 3,
 ( #5178, #5362, #8569, #6075, #6027, #7920 ),
 .UNSPECIFIED., .F., .F.,
 ( 4, 2, 4 ),
 ( 2.380731626890628072E-07, 0.002336973833157054200, 0.004673709593151418457 ),
 .UNSPECIFIED. ) ;
#2892 = DIRECTION ( 'NONE',  ( -3.851859888774471706E-33, -1.232595164407830946E-32, -1.000000000000000000 ) ) ;
#2893 = ORIENTED_EDGE ( 'NONE', *, *, #5359, .F. ) ;
#2894 = DIRECTION ( 'NONE',  ( 3.851859888774471706E-33, 1.232595164407830946E-32, 1.000000000000000000 ) ) ;
#2895 = DIRECTION ( 'NONE',  ( -1.000000000000000000, -8.881784197001244435E-16, 0.000000000000000000 ) ) ;
#2896 = CYLINDRICAL_SURFACE ( 'NONE', #3922, 5.559999999999998721 ) ;
#2897 = ORIENTED_EDGE ( 'NONE', *, *, #571, .T. ) ;
#2898 = ORIENTED_EDGE ( 'NONE', *, *, #592, .T. ) ;
#2899 = ORIENTED_EDGE ( 'NONE', *, *, #2331, .T. ) ;
#2900 = CYLINDRICAL_SURFACE ( 'NONE', #2262, 5.749999999999991118 ) ;
#2901 = LINE ( 'NONE', #7568, #8115 ) ;
#2902 = CARTESIAN_POINT ( 'NONE',  ( -17.49999999999955236, 120.0000000000003268, 9.999999999999980460 ) ) ;
#2903 = CARTESIAN_POINT ( 'NONE',  ( 4.000000000000003553, -1.759474945355333109, 3.047500000000091802 ) ) ;
#2904 = CARTESIAN_POINT ( 'NONE',  ( -8.000000000000007105, -4.618802153517398423, -7.685468820183672278 ) ) ;
#2905 = AXIS2_PLACEMENT_3D ( 'NONE', #1433, #4045, #2604 ) ;
#2906 = FACE_OUTER_BOUND ( 'NONE', #2768, .T. ) ;
#2907 = ORIENTED_EDGE ( 'NONE', *, *, #4501, .F. ) ;
#2908 = AXIS2_PLACEMENT_3D ( 'NONE', #7026, #3716, #6298 ) ;
#2909 = DIRECTION ( 'NONE',  ( 0.000000000000000000, -0.4999999999999983902, 0.8660254037844395958 ) ) ;
#2910 = EDGE_LOOP ( 'NONE', ( #6899, #6956, #7499, #73 ) ) ;
#2911 = VECTOR ( 'NONE', #1096, 1000.000000000000000 ) ;
#2912 = EDGE_CURVE ( 'NONE', #1989, #2069, #3630, .T. ) ;
#2913 = AXIS2_PLACEMENT_3D ( 'NONE', #1332, #1895, #3941 ) ;
#2914 = DIRECTION ( 'NONE',  ( 1.000000000000000000, 0.000000000000000000, 0.000000000000000000 ) ) ;
#2915 = ORIENTED_EDGE ( 'NONE', *, *, #2653, .F. ) ;
#2916 = B_SPLINE_CURVE_WITH_KNOTS ( 'NONE', 3,
 ( #8046, #4612, #2084, #7260, #4743, #8410 ),
 .UNSPECIFIED., .F., .F.,
 ( 4, 2, 4 ),
 ( 2.380731630570001552E-07, 0.002336973833157701252, 0.004673709593152344799 ),
 .UNSPECIFIED. ) ;
#2917 = CARTESIAN_POINT ( 'NONE',  ( 10.00000000000000888, -0.8578643762688908936, -20.00000000000001776 ) ) ;
#2918 = ORIENTED_EDGE ( 'NONE', *, *, #3859, .T. ) ;
#2919 = CIRCLE ( 'NONE', #1799, 39.99999999999999289 ) ;
#2920 = ORIENTED_EDGE ( 'NONE', *, *, #445, .T. ) ;
#2921 = CIRCLE ( 'NONE', #1400, 5.749999999999985789 ) ;
#2922 = CIRCLE ( 'NONE', #6406, 14.99999999999987388 ) ;
#2923 = CIRCLE ( 'NONE', #7239, 3.047499999999999876 ) ;
#2924 = EDGE_CURVE ( 'NONE', #1524, #4837, #2952, .T. ) ;
#2925 = DIRECTION ( 'NONE',  ( -1.463706757734299248E-32, 1.000000000000000000, 5.238529448733281520E-32 ) ) ;
#2926 = AXIS2_PLACEMENT_3D ( 'NONE', #3575, #8181, #1726 ) ;
#2927 = DIRECTION ( 'NONE',  ( -1.000000000000000000, 0.000000000000000000, 6.938893903907228378E-17 ) ) ;
#2928 = ORIENTED_EDGE ( 'NONE', *, *, #1734, .F. ) ;
#2929 = CARTESIAN_POINT ( 'NONE',  ( 1.110223024625156540E-13, -414.9999999999999432, 19.49999999999989342 ) ) ;
#2930 = DIRECTION ( 'NONE',  ( 1.718667387362693737E-17, -0.9879598069184307718, -0.1547107621133612942 ) ) ;
#2931 = VERTEX_POINT ( 'NONE', #4996 ) ;
#2932 = DIRECTION ( 'NONE',  ( 0.000000000000000000, 0.000000000000000000, 1.000000000000000000 ) ) ;
#2933 = B_SPLINE_CURVE_WITH_KNOTS ( 'NONE', 3,
 ( #1810, #1156, #5158, #7815, #635, #6693 ),
 .UNSPECIFIED., .F., .F.,
 ( 4, 2, 4 ),
 ( 2.380731631918482768E-07, 0.002336973833157790156, 0.004673709593152389034 ),
 .UNSPECIFIED. ) ;
#2934 = EDGE_LOOP ( 'NONE', ( #5981, #8102, #1693, #399 ) ) ;
#2935 = CARTESIAN_POINT ( 'NONE',  ( 4.250000000000000888, 32.50000000000005684, 18.00000000000000355 ) ) ;
#2936 = ADVANCED_FACE ( 'NONE', ( #7662 ), #3342, .T. ) ;
#2937 = CARTESIAN_POINT ( 'NONE',  ( 0.000000000000000000, 0.000000000000000000, -8.400000000000018119 ) ) ;
#2938 = VERTEX_POINT ( 'NONE', #8399 ) ;
#2939 = CARTESIAN_POINT ( 'NONE',  ( 7.347286611336957485, 4.995646404165022147, -0.4969600502616601245 ) ) ;
#2940 = ORIENTED_EDGE ( 'NONE', *, *, #4022, .F. ) ;
#2941 = MECHANICAL_DESIGN_GEOMETRIC_PRESENTATION_REPRESENTATION (  '', ( #2252 ), #1423 ) ;
#2942 = ADVANCED_FACE ( 'NONE', ( #4608 ), #5117, .F. ) ;
#2943 = DIRECTION ( 'NONE',  ( -1.463706757734299248E-32, 1.000000000000000000, 5.238529448733281520E-32 ) ) ;
#2944 = ORIENTED_EDGE ( 'NONE', *, *, #6930, .F. ) ;
#2945 = ORIENTED_EDGE ( 'NONE', *, *, #805, .F. ) ;
#2946 = MANIFOLD_SOLID_BREP ( 'Chamfer1', #4312 ) ;
#2947 = DIRECTION ( 'NONE',  ( 1.000000000000000000, 8.881784197001244435E-16, 0.000000000000000000 ) ) ;
#2948 = CARTESIAN_POINT ( 'NONE',  ( 0.000000000000000000, 0.000000000000000000, 0.000000000000000000 ) ) ;
#2949 = LINE ( 'NONE', #1676, #4319 ) ;
#2950 = VERTEX_POINT ( 'NONE', #7257 ) ;
#2951 = EDGE_CURVE ( 'NONE', #4496, #4055, #1811, .T. ) ;
#2952 = LINE ( 'NONE', #5635, #141 ) ;
#2953 = VERTEX_POINT ( 'NONE', #6403 ) ;
#2954 = AXIS2_PLACEMENT_3D ( 'NONE', #7903, #8550, #7383 ) ;
#2955 = CIRCLE ( 'NONE', #6995, 5.499999999999999112 ) ;
#2956 = CIRCLE ( 'NONE', #1975, 4.250000000000010658 ) ;
#2957 = CIRCLE ( 'NONE', #176, 5.500000000000024869 ) ;
#2958 = DIRECTION ( 'NONE',  ( 0.000000000000000000, 0.000000000000000000, -1.000000000000000000 ) ) ;
#2959 = VERTEX_POINT ( 'NONE', #7738 ) ;
#2960 = CARTESIAN_POINT ( 'NONE',  ( 5.000000000000004441, 0.000000000000000000, 0.000000000000000000 ) ) ;
#2961 = ORIENTED_EDGE ( 'NONE', *, *, #3356, .F. ) ;
#2962 = B_SPLINE_CURVE_WITH_KNOTS ( 'NONE', 3,
 ( #7773, #5076, #1195, #5722, #7170, #5114 ),
 .UNSPECIFIED., .F., .F.,
 ( 4, 2, 4 ),
 ( 0.01291313371729433702, 0.01525081363757293043, 0.01758849355785152557 ),
 .UNSPECIFIED. ) ;
#2963 = MANIFOLD_SOLID_BREP ( 'Boss-Extrude1', #7516 ) ;
#2964 = CONICAL_SURFACE ( 'NONE', #1439, 8.000000000000007105, 1.047197551196597631 ) ;
#2965 = ORIENTED_EDGE ( 'NONE', *, *, #7217, .T. ) ;
#2966 = EDGE_CURVE ( 'NONE', #1504, #7258, #1859, .T. ) ;
#2967 = DIRECTION ( 'NONE',  ( 4.622231866529366047E-33, -1.224646799147353454E-16, 1.000000000000000000 ) ) ;
#2968 = AXIS2_PLACEMENT_3D ( 'NONE', #1092, #3052, #8369 ) ;
#2969 = CARTESIAN_POINT ( 'NONE',  ( 4.000000000000003553, 6.928203230275597591, -8.400000000000018119 ) ) ;
#2970 = CARTESIAN_POINT ( 'NONE',  ( 5.690023276062378343, 5.952467836904126841, -0.1306530452037925616 ) ) ;
#2971 = VERTEX_POINT ( 'NONE', #7438 ) ;
#2972 = AXIS2_PLACEMENT_3D ( 'NONE', #1599, #869, #2997 ) ;
#2973 = PLANE ( 'NONE',  #2665 ) ;
#2974 = ADVANCED_FACE ( 'NONE', ( #4083 ), #6065, .T. ) ;
#2975 = AXIS2_PLACEMENT_3D ( 'NONE', #3618, #4959, #4311 ) ;
#2976 = CARTESIAN_POINT ( 'NONE',  ( -8.000000000000005329, 1.572549600175600970, -8.331055444744887239 ) ) ;
#2977 = DIRECTION ( 'NONE',  ( 1.000000000000000000, -5.898059818321089887E-17, -4.579669976578770729E-16 ) ) ;
#2978 = VERTEX_POINT ( 'NONE', #3338 ) ;
#2979 = CARTESIAN_POINT ( 'NONE',  ( 0.000000000000000000, 32.50000000000005684, 18.00000000000000355 ) ) ;
#2980 = MANIFOLD_SOLID_BREP ( 'Extrude-Thin1', #6001 ) ;
#2981 = ORIENTED_EDGE ( 'NONE', *, *, #4888, .T. ) ;
#2982 = CARTESIAN_POINT ( 'NONE',  ( 275.0000000000000000, -425.0000000000000000, 0.000000000000000000 ) ) ;
#2983 = CARTESIAN_POINT ( 'NONE',  ( 1.110223024625156540E-13, -414.9999999999999432, -6.938893903907228378E-14 ) ) ;
#2984 = FACE_OUTER_BOUND ( 'NONE', #4206, .T. ) ;
#2985 = ORIENTED_EDGE ( 'NONE', *, *, #2395, .T. ) ;
#2986 = DIRECTION ( 'NONE',  ( 0.000000000000000000, 1.540743955509787842E-29, -1.000000000000000000 ) ) ;
#2987 = EDGE_CURVE ( 'NONE', #3472, #6642, #8000, .T. ) ;
#2988 = EDGE_CURVE ( 'NONE', #650, #2856, #5832, .T. ) ;
#2989 = EDGE_LOOP ( 'NONE', ( #8204, #85, #2807, #2625 ) ) ;
#2990 = ORIENTED_EDGE ( 'NONE', *, *, #4325, .F. ) ;
#2991 = VECTOR ( 'NONE', #8366, 1000.000000000000000 ) ;
#2992 = CARTESIAN_POINT ( 'NONE',  ( 8.000000000000007105, -4.618802153517121312, -7.685468820183672278 ) ) ;
#2993 = ADVANCED_FACE ( 'NONE', ( #773 ), #5144, .T. ) ;
#2994 = CIRCLE ( 'NONE', #6770, 8.000000000000007105 ) ;
#2995 = CARTESIAN_POINT ( 'NONE',  ( 0.000000000000000000, 0.000000000000000000, 0.000000000000000000 ) ) ;
#2996 = CARTESIAN_POINT ( 'NONE',  ( 3.999999999999337419, -6.928203230275431501, -8.400000000000018119 ) ) ;
#2997 = DIRECTION ( 'NONE',  ( 6.400024471206997542E-36, -1.000000000000000000, -7.598173571352216173E-18 ) ) ;
#2998 = ORIENTED_EDGE ( 'NONE', *, *, #8586, .F. ) ;
#2999 = LINE ( 'NONE', #249, #2366 ) ;
#3000 = ORIENTED_EDGE ( 'NONE', *, *, #3291, .F. ) ;
#3001 = CARTESIAN_POINT ( 'NONE',  ( 0.000000000000000000, 415.0000000000000000, -5.551115123125782702E-14 ) ) ;
#3002 = DIRECTION ( 'NONE',  ( -7.703719777548943412E-34, 0.000000000000000000, 1.000000000000000000 ) ) ;
#3003 = VERTEX_POINT ( 'NONE', #2692 ) ;
#3004 = AXIS2_PLACEMENT_3D ( 'NONE', #2948, #2138, #6797 ) ;
#3005 = EDGE_LOOP ( 'NONE', ( #3658, #8012, #2985, #5669 ) ) ;
#3006 = CARTESIAN_POINT ( 'NONE',  ( 0.000000000000000000, 0.000000000000000000, -8.400000000000018119 ) ) ;
#3007 = CARTESIAN_POINT ( 'NONE',  ( 0.000000000000000000, -32.50000000000004974, 18.00000000000000355 ) ) ;
#3008 = PRODUCT_DEFINITION ( 'UNKNOWN', '', #3962, #8224 ) ;
#3009 = AXIS2_PLACEMENT_3D ( 'NONE', #814, #6696, #859 ) ;
#3010 = CARTESIAN_POINT ( 'NONE',  ( 7.999999999999674039, -4.618802153517231446, -0.7145311798163467287 ) ) ;
#3011 = ORIENTED_EDGE ( 'NONE', *, *, #7073, .T. ) ;
#3012 = LINE ( 'NONE', #7112, #2911 ) ;
#3013 = VECTOR ( 'NONE', #5841, 1000.000000000000000 ) ;
#3014 = CARTESIAN_POINT ( 'NONE',  ( 50.00000000000004263, 500.0000000000000000, 50.00000000000000000 ) ) ;
#3015 = DIRECTION ( 'NONE',  ( -4.579669976578766785E-16, -5.898059818321121934E-17, -1.000000000000000000 ) ) ;
#3016 = ORIENTED_EDGE ( 'NONE', *, *, #930, .F. ) ;
#3017 = FACE_OUTER_BOUND ( 'NONE', #46, .T. ) ;
#3018 = CARTESIAN_POINT ( 'NONE',  ( 8.400000000000018119, -5.497230663963303402E-14, 4.400000000000696687 ) ) ;
#3019 = EDGE_CURVE ( 'NONE', #2145, #282, #8002, .T. ) ;
#3020 = DIRECTION ( 'NONE',  ( 7.703719777548943412E-34, -0.000000000000000000, -1.000000000000000000 ) ) ;
#3021 = ORIENTED_EDGE ( 'NONE', *, *, #769, .T. ) ;
#3022 = CARTESIAN_POINT ( 'NONE',  ( 8.000000000000120792, 1.572549600175473739, -8.331055444744837502 ) ) ;
#3023 = DIRECTION ( 'NONE',  ( -1.000000000000000000, 1.774937036747276562E-30, 0.000000000000000000 ) ) ;
#3024 = SHAPE_REPRESENTATION_RELATIONSHIP ( 'NONE' , 'NONE' ,  #7270, #3221 ) ;
#3025 = EDGE_LOOP ( 'NONE', ( #4964, #1957, #4715 ) ) ;
#3026 = ORIENTED_EDGE ( 'NONE', *, *, #8231, .F. ) ;
#3027 = FACE_OUTER_BOUND ( 'NONE', #861, .T. ) ;
#3028 = ORIENTED_EDGE ( 'NONE', *, *, #1979, .F. ) ;
#3029 = LINE ( 'NONE', #1628, #8246 ) ;
#3030 = APPLICATION_CONTEXT ( 'automotive_design' ) ;
#3031 = EDGE_CURVE ( 'NONE', #6260, #6357, #3633, .T. ) ;
#3032 = CARTESIAN_POINT ( 'NONE',  ( -8.000000000000671463, 1.572549600175901618, -8.331055444744475125 ) ) ;
#3033 = CARTESIAN_POINT ( 'NONE',  ( 0.000000000000000000, 0.000000000000000000, 0.000000000000000000 ) ) ;
#3034 = CARTESIAN_POINT ( 'NONE',  ( 0.000000000000000000, 299.9999999999999432, -70.00000000000015632 ) ) ;
#3035 = DIRECTION ( 'NONE',  ( 0.000000000000000000, -0.000000000000000000, 1.000000000000000000 ) ) ;
#3036 = DIRECTION ( 'NONE',  ( 1.000000000000000000, 0.000000000000000000, 0.000000000000000000 ) ) ;
#3037 = EDGE_LOOP ( 'NONE', ( #1291, #1169, #881, #8078, #1665, #94 ) ) ;
#3038 = DIRECTION ( 'NONE',  ( 3.851859888774471706E-33, -7.598173571352216173E-18, 1.000000000000000000 ) ) ;
#3039 = ORIENTED_EDGE ( 'NONE', *, *, #7605, .T. ) ;
#3040 = AXIS2_PLACEMENT_3D ( 'NONE', #4180, #8187, #1249 ) ;
#3041 = EDGE_CURVE ( 'NONE', #2313, #2221, #993, .T. ) ;
#3042 = CARTESIAN_POINT ( 'NONE',  ( 0.000000000000000000, 0.000000000000000000, 0.000000000000000000 ) ) ;
#3043 = ADVANCED_FACE ( 'NONE', ( #8134, #727, #4738, #2175, #4822, #1336, #1290, #3948 ), #639, .T. ) ;
#3044 = CIRCLE ( 'NONE', #4155, 4.499999999999983125 ) ;
#3045 = FACE_BOUND ( 'NONE', #8495, .T. ) ;
#3046 = VERTEX_POINT ( 'NONE', #5570 ) ;
#3047 = ORIENTED_EDGE ( 'NONE', *, *, #7195, .F. ) ;
#3048 = LINE ( 'NONE', #5736, #2991 ) ;
#3049 = ADVANCED_FACE ( 'NONE', ( #4859 ), #730, .T. ) ;
#3050 = AXIS2_PLACEMENT_3D ( 'NONE', #1237, #96, #6060 ) ;
#3051 = UNCERTAINTY_MEASURE_WITH_UNIT (LENGTH_MEASURE( 1.000000000000000082E-05 ), #945, 'distance_accuracy_value', 'NONE');
#3052 = DIRECTION ( 'NONE',  ( -1.000000000000000000, 3.549874073494553124E-30, 0.000000000000000000 ) ) ;
#3053 = PLANE ( 'NONE',  #8241 ) ;
#3054 = CARTESIAN_POINT ( 'NONE',  ( -85.74999999999972999, 15.00000000000010836, 1.942890293094023693E-13 ) ) ;
#3055 = ORIENTED_EDGE ( 'NONE', *, *, #5043, .T. ) ;
#3056 = AXIS2_PLACEMENT_3D ( 'NONE', #7069, #4328, #4971 ) ;
#3057 = CARTESIAN_POINT ( 'NONE',  ( 4.339467034331248918, 6.732211846623395779, -8.400000000000000355 ) ) ;
#3058 = PRODUCT_DEFINITION_SHAPE ( 'NONE', 'NONE',  #5591 ) ;
#3059 = DIRECTION ( 'NONE',  ( -6.400024471207001551E-36, 1.000000000000000000, 7.598173571352213092E-18 ) ) ;
#3060 = DIRECTION ( 'NONE',  ( 1.000000000000000000, -5.898059818321126865E-17, -4.579669976578766785E-16 ) ) ;
#3061 = ADVANCED_FACE ( 'NONE', ( #2327 ), #2247, .T. ) ;
#3062 = CARTESIAN_POINT ( 'NONE',  ( 4.000000000000003553, 9.714451465470119729E-14, 0.000000000000000000 ) ) ;
#3063 = CIRCLE ( 'NONE', #4449, 8.000000000000007105 ) ;
#3064 = DIRECTION ( 'NONE',  ( 3.851859888774471706E-33, 1.232595164407830946E-32, 1.000000000000000000 ) ) ;
#3065 = ORIENTED_EDGE ( 'NONE', *, *, #5225, .F. ) ;
#3066 = LINE ( 'NONE', #7118, #3329 ) ;
#3067 =( NAMED_UNIT ( * ) SI_UNIT ( $, .STERADIAN. ) SOLID_ANGLE_UNIT ( ) );
#3068 = ORIENTED_EDGE ( 'NONE', *, *, #3170, .F. ) ;
#3069 = EDGE_CURVE ( 'NONE', #3768, #748, #4983, .T. ) ;
#3070 = LINE ( 'NONE', #421, #6723 ) ;
#3071 = ORIENTED_EDGE ( 'NONE', *, *, #2570, .F. ) ;
#3072 = LINE ( 'NONE', #7080, #4481 ) ;
#3073 = CARTESIAN_POINT ( 'NONE',  ( -8.000000000000667910, 0.7809653281580535289, -8.399999999999606004 ) ) ;
#3074 = CARTESIAN_POINT ( 'NONE',  ( 0.000000000000000000, -1.759474945355326225, -3.047499999999869758 ) ) ;
#3075 = CARTESIAN_POINT ( 'NONE',  ( 4.000000000000003553, -6.928203230275542523, -8.400000000000018119 ) ) ;
#3076 = CARTESIAN_POINT ( 'NONE',  ( -3.318518101603131765, -7.321656987762887425, -3.464364754270089018E-14 ) ) ;
#3077 =( REPRESENTATION_RELATIONSHIP ('NONE','NONE', #1279, #7270 ) REPRESENTATION_RELATIONSHIP_WITH_TRANSFORMATION ( #7097 )SHAPE_REPRESENTATION_RELATIONSHIP( ) );
#3078 = CARTESIAN_POINT ( 'NONE',  ( 0.000000000000000000, -29.14213562373091548, 79.99999999999995737 ) ) ;
#3079 = EDGE_LOOP ( 'NONE', ( #2852, #1757, #6501, #630, #284, #2048, #8486, #7214, #4382 ) ) ;
#3080 = ADVANCED_FACE ( 'NONE', ( #8264 ), #994, .T. ) ;
#3081 = CARTESIAN_POINT ( 'NONE',  ( 4.000000000000003553, 6.928203230275597591, 0.000000000000000000 ) ) ;
#3082 = ORIENTED_EDGE ( 'NONE', *, *, #8370, .F. ) ;
#3083 = DIRECTION ( 'NONE',  ( -1.000000000000000000, 1.774937036747276562E-30, 0.000000000000000000 ) ) ;
#3084 = PLANE ( 'NONE',  #4433 ) ;
#3085 = ORIENTED_EDGE ( 'NONE', *, *, #1190, .F. ) ;
#3086 = AXIS2_PLACEMENT_3D ( 'NONE', #4302, #5579, #8227 ) ;
#3087 = DIRECTION ( 'NONE',  ( -0.000000000000000000, -0.000000000000000000, 1.000000000000000000 ) ) ;
#3088 = ADVANCED_FACE ( 'NONE', ( #3867 ), #4666, .F. ) ;
#3089 = AXIS2_PLACEMENT_3D ( 'NONE', #1582, #4894, #8083 ) ;
#3090 = LINE ( 'NONE', #1688, #6449 ) ;
#3091 = AXIS2_PLACEMENT_3D ( 'NONE', #2102, #657, #8020 ) ;
#3092 = VECTOR ( 'NONE', #5383, 1000.000000000000000 ) ;
#3093 = LINE ( 'NONE', #3873, #4209 ) ;
#3094 = ORIENTED_EDGE ( 'NONE', *, *, #5793, .T. ) ;
#3095 = AXIS2_PLACEMENT_3D ( 'NONE', #1702, #6951, #7718 ) ;
#3096 = CARTESIAN_POINT ( 'NONE',  ( 6.689127551062064470, 5.375634714784610857, -8.082649155111342409 ) ) ;
#3097 = CARTESIAN_POINT ( 'NONE',  ( 139.9999999999994316, 3.469446951953614189E-14, -1.443289932012703503E-12 ) ) ;
#3098 = AXIS2_PLACEMENT_3D ( 'NONE', #1964, #703, #7279 ) ;
#3099 = CIRCLE ( 'NONE', #4222, 8.000000000000007105 ) ;
#3100 = CYLINDRICAL_SURFACE ( 'NONE', #4489, 75.00000000000000000 ) ;
#3101 = AXIS2_PLACEMENT_3D ( 'NONE', #5695, #2308, #447 ) ;
#3102 = AXIS2_PLACEMENT_3D ( 'NONE', #5160, #7818, #5891 ) ;
#3103 = ADVANCED_FACE ( 'NONE', ( #1255 ), #3351, .F. ) ;
#3104 = CARTESIAN_POINT ( 'NONE',  ( 0.000000000000000000, 60.00000000000000000, -50.00000000000000000 ) ) ;
#3105 = VERTEX_POINT ( 'NONE', #2706 ) ;
#3106 = CIRCLE ( 'NONE', #7421, 80.00000000000001421 ) ;
#3107 = ADVANCED_FACE ( 'NONE', ( #6710 ), #6719, .F. ) ;
#3108 = LINE ( 'NONE', #1185, #8070 ) ;
#3109 = VERTEX_POINT ( 'NONE', #611 ) ;
#3110 = CIRCLE ( 'NONE', #4628, 14.99999999999987388 ) ;
#3111 = CARTESIAN_POINT ( 'NONE',  ( -2.309976723937442689, 7.903938623646887152, -0.1306530452037944767 ) ) ;
#3112 = ORIENTED_EDGE ( 'NONE', *, *, #7757, .T. ) ;
#3113 = DIRECTION ( 'NONE',  ( 0.000000000000000000, -0.5000000000000009992, -0.8660254037844380415 ) ) ;
#3114 = DIRECTION ( 'NONE',  ( 8.659560562354746736E-17, -0.7071067811865321406, -0.7071067811865628938 ) ) ;
#3115 =( REPRESENTATION_RELATIONSHIP ('NONE','NONE', #1279, #6969 ) REPRESENTATION_RELATIONSHIP_WITH_TRANSFORMATION ( #6660 )SHAPE_REPRESENTATION_RELATIONSHIP( ) );
#3116 = EDGE_CURVE ( 'NONE', #8386, #8336, #2660, .T. ) ;
#3117 = PLANE ( 'NONE',  #5090 ) ;
#3118 = PRODUCT_DEFINITION ( 'UNKNOWN', '', #4508, #1593 ) ;
#3119 = PRODUCT_DEFINITION_FORMATION_WITH_SPECIFIED_SOURCE ( 'ANY', '', #2728, .NOT_KNOWN. ) ;
#3120 = SURFACE_STYLE_USAGE ( .BOTH. , #7692 ) ;
#3121 = DIRECTION ( 'NONE',  ( 0.7071067811865483499, 8.659560562353920898E-17, 0.7071067811865467956 ) ) ;
#3122 = DIRECTION ( 'NONE',  ( -1.000000000000000000, 3.549874073494553124E-30, 0.000000000000000000 ) ) ;
#3123 = FACE_OUTER_BOUND ( 'NONE', #6717, .T. ) ;
#3124 = EDGE_LOOP ( 'NONE', ( #5831, #1557, #5683, #7930 ) ) ;
#3125 = SURFACE_STYLE_FILL_AREA ( #3783 ) ;
#3126 = VERTEX_POINT ( 'NONE', #4050 ) ;
#3127 = FACE_OUTER_BOUND ( 'NONE', #6595, .T. ) ;
#3128 = ADVANCED_FACE ( 'NONE', ( #3911, #6574 ), #8530, .T. ) ;
#3129 = VECTOR ( 'NONE', #2425, 1000.000000000000000 ) ;
#3130 = CONTEXT_DEPENDENT_SHAPE_REPRESENTATION ( #3077, #5372 ) ;
#3131 = CARTESIAN_POINT ( 'NONE',  ( 1.313474075706796862, 8.479269695851089139, -8.083279549040090828 ) ) ;
#3132 = EDGE_LOOP ( 'NONE', ( #6247, #4922, #607, #7004 ) ) ;
#3133 = ORIENTED_EDGE ( 'NONE', *, *, #1714, .F. ) ;
#3134 = DIRECTION ( 'NONE',  ( 0.000000000000000000, -1.000000000000000000, -7.598173571352319403E-18 ) ) ;
#3135 = DIRECTION ( 'NONE',  ( 3.919652622816902408E-30, 3.944304526105059027E-30, -1.000000000000000000 ) ) ;
#3136 = EDGE_CURVE ( 'NONE', #2816, #5332, #2956, .T. ) ;
#3137 = FACE_OUTER_BOUND ( 'NONE', #7878, .T. ) ;
#3138 = CARTESIAN_POINT ( 'NONE',  ( 1.110223024625156540E-13, -410.0000000000000568, -6.938893903907228378E-14 ) ) ;
#3139 = VERTEX_POINT ( 'NONE', #6667 ) ;
#3140 = DIRECTION ( 'NONE',  ( -0.000000000000000000, -0.000000000000000000, 1.000000000000000000 ) ) ;
#3141 = CARTESIAN_POINT ( 'NONE',  ( 20.00000000000011724, -14.99999999999990230, -20.00000000000001776 ) ) ;
#3142 = CARTESIAN_POINT ( 'NONE',  ( -7.999999999999785061, 4.618802153516954334, -7.685468820183672278 ) ) ;
#3143 = DIRECTION ( 'NONE',  ( -1.058471975245261993E-16, 8.736544766236848795E-16, -1.000000000000000000 ) ) ;
#3144 = ADVANCED_BREP_SHAPE_REPRESENTATION ( '', ( #20, #7563 ), #4918 ) ;
#3145 = EDGE_CURVE ( 'NONE', #8513, #4401, #2891, .T. ) ;
#3146 = EDGE_CURVE ( 'NONE', #3833, #2054, #1278, .T. ) ;
#3147 = CARTESIAN_POINT ( 'NONE',  ( 1.110223024625156540E-13, 9.237604307033992157, -0.7145311798163467287 ) ) ;
#3148 = EDGE_LOOP ( 'NONE', ( #4973, #8440, #2189, #2676 ) ) ;
#3149 = CIRCLE ( 'NONE', #1344, 5.499999999999999112 ) ;
#3150 = DIRECTION ( 'NONE',  ( 1.000000000000000000, 2.775557561562898056E-15, -3.821045009664285041E-30 ) ) ;
#3151 =( LENGTH_UNIT ( ) NAMED_UNIT ( * ) SI_UNIT ( .MILLI., .METRE. ) );
#3152 = ORIENTED_EDGE ( 'NONE', *, *, #2132, .F. ) ;
#3153 = SURFACE_STYLE_USAGE ( .BOTH. , #1925 ) ;
#3154 = EDGE_CURVE ( 'NONE', #8100, #6175, #7314, .T. ) ;
#3155 = CARTESIAN_POINT ( 'NONE',  ( -3.319543390095889723, 7.321065037175431556, -0.01688885742773474710 ) ) ;
#3156 = ORIENTED_EDGE ( 'NONE', *, *, #3840, .T. ) ;
#3157 = CARTESIAN_POINT ( 'NONE',  ( 4.000000000000114575, 6.928203230275597591, -8.400000000000018119 ) ) ;
#3158 = CONICAL_SURFACE ( 'NONE', #7067, 9.499999999999998224, 0.7853981633974257415 ) ;
#3159 = AXIS2_PLACEMENT_3D ( 'NONE', #1918, #4576, #7231 ) ;
#3160 = CARTESIAN_POINT ( 'NONE',  ( -8.000000000000673239, 3.871967595402326268, -7.901061386767160855 ) ) ;
#3161 = CARTESIAN_POINT ( 'NONE',  ( -8.000000000000007105, -4.618802153517398423, -0.7145311798163467287 ) ) ;
#3162 = DIRECTION ( 'NONE',  ( 1.000000000000000000, 0.000000000000000000, -5.478200730701491345E-30 ) ) ;
#3163 = CARTESIAN_POINT ( 'NONE',  ( -4.680456609904036114, -6.535341423375559344, -8.383111142572246877 ) ) ;
#3164 = FACE_BOUND ( 'NONE', #7637, .T. ) ;
#3165 = CARTESIAN_POINT ( 'NONE',  ( -3.319543390095888835, 7.321065037175429779, -8.383111142572282404 ) ) ;
#3166 = ORIENTED_EDGE ( 'NONE', *, *, #1936, .F. ) ;
#3167 = SHAPE_REPRESENTATION ( 'hex nut style 1_am_B18.2.4.1M - Hex nut, Style 1,  M10 x 1.5, with 16mm WAF --D-N', ( #7563 ), #1720 ) ;
#3168 = CIRCLE ( 'NONE', #5399, 8.000000000000007105 ) ;
#3169 = EDGE_LOOP ( 'NONE', ( #381, #1517, #7092, #4001 ) ) ;
#3170 = EDGE_CURVE ( 'NONE', #3105, #2011, #8405, .T. ) ;
#3171 = DIRECTION ( 'NONE',  ( -1.463706757734299248E-32, 1.000000000000000000, 5.238529448733281520E-32 ) ) ;
#3172 = CARTESIAN_POINT ( 'NONE',  ( 5.000000000000115463, -14.99999999999990230, 79.99999999999995737 ) ) ;
#3173 = EDGE_LOOP ( 'NONE', ( #962, #196 ) ) ;
#3174 = DIRECTION ( 'NONE',  ( 6.400024471206997542E-36, -1.000000000000000000, 0.000000000000000000 ) ) ;
#3175 = ORIENTED_EDGE ( 'NONE', *, *, #2051, .T. ) ;
#3176 = EDGE_CURVE ( 'NONE', #79, #1769, #2609, .T. ) ;
#3177 = CARTESIAN_POINT ( 'NONE',  ( -6.689127551062228783, -5.375634714784562895, -8.082649155111287342 ) ) ;
#3178 = CIRCLE ( 'NONE', #4297, 8.000000000000007105 ) ;
#3179 = FACE_OUTER_BOUND ( 'NONE', #4897, .T. ) ;
#3180 = LINE ( 'NONE', #2531, #8114 ) ;
#3181 = EDGE_LOOP ( 'NONE', ( #7921, #2760, #2323, #2595, #504, #3000 ) ) ;
#3182 = DIRECTION ( 'NONE',  ( 1.000000000000000000, 8.736544766236848795E-16, -1.058471975245254351E-16 ) ) ;
#3183 = AXIS2_PLACEMENT_3D ( 'NONE', #4392, #2376, #7732 ) ;
#3184 = EDGE_CURVE ( 'NONE', #5903, #8505, #2063, .T. ) ;
#3185 = CARTESIAN_POINT ( 'NONE',  ( 5.000000000000060396, -4.857225732735079428E-14, -4.057500000000047180 ) ) ;
#3186 = ORIENTED_EDGE ( 'NONE', *, *, #7417, .T. ) ;
#3187 = DIRECTION ( 'NONE',  ( -1.000000000000000000, 3.549874073494553124E-30, 0.000000000000000000 ) ) ;
#3188 = AXIS2_PLACEMENT_3D ( 'NONE', #1236, #4691, #3895 ) ;
#3189 = AXIS2_PLACEMENT_3D ( 'NONE', #4974, #2695, #3385 ) ;
#3190 = AXIS2_PLACEMENT_3D ( 'NONE', #2413, #8300, #2452 ) ;
#3191 = DIRECTION ( 'NONE',  ( -0.000000000000000000, -1.000000000000000000, -1.795949010423047374E-16 ) ) ;
#3192 = VERTEX_POINT ( 'NONE', #1308 ) ;
#3193 = EDGE_CURVE ( 'NONE', #4094, #5811, #3304, .T. ) ;
#3194 = DIRECTION ( 'NONE',  ( -0.000000000000000000, -0.000000000000000000, 1.000000000000000000 ) ) ;
#3195 = PRODUCT ( 'Motor mount pad', 'Motor mount pad', '', ( #2713 ) ) ;
#3196 = VERTEX_POINT ( 'NONE', #787 ) ;
#3197 = CARTESIAN_POINT ( 'NONE',  ( 5.690023276062460056, 5.952467836904209442, -8.269346954796159110 ) ) ;
#3198 = COLOUR_RGB ( '',0.7921568627450980005, 0.8196078431372548767, 0.9333333333333333481 ) ;
#3199 = CARTESIAN_POINT ( 'NONE',  ( -50.00000000000004263, 500.0000000000000000, -50.00000000000000000 ) ) ;
#3200 = LINE ( 'NONE', #4552, #1686 ) ;
#3201 = FACE_OUTER_BOUND ( 'NONE', #5224, .T. ) ;
#3202 = EDGE_CURVE ( 'NONE', #4479, #2931, #581, .T. ) ;
#3203 = CARTESIAN_POINT ( 'NONE',  ( 0.000000000000000000, 0.000000000000000000, -45.00000000000000711 ) ) ;
#3204 = DIRECTION ( 'NONE',  ( 0.000000000000000000, -5.322451846059955323E-30, 1.000000000000000000 ) ) ;
#3205 = ORIENTED_EDGE ( 'NONE', *, *, #3280, .T. ) ;
#3206 = SURFACE_SIDE_STYLE ('',( #3125 ) ) ;
#3207 = ORIENTED_EDGE ( 'NONE', *, *, #7936, .F. ) ;
#3208 = CARTESIAN_POINT ( 'NONE',  ( 5.000000000000004441, 0.000000000000000000, 0.000000000000000000 ) ) ;
#3209 = AXIS2_PLACEMENT_3D ( 'NONE', #6419, #8327, #1829 ) ;
#3210 = CARTESIAN_POINT ( 'NONE',  ( 139.9999999999994316, 3.469446951953614189E-14, -1.443289932012703503E-12 ) ) ;
#3211 =( NAMED_UNIT ( * ) SI_UNIT ( $, .STERADIAN. ) SOLID_ANGLE_UNIT ( ) );
#3212 = VECTOR ( 'NONE', #4535, 1000.000000000000000 ) ;
#3213 = CARTESIAN_POINT ( 'NONE',  ( 7.345652830558279334, -4.996589667937374024, -7.903584543331455770 ) ) ;
#3214 = PLANE ( 'NONE',  #4107 ) ;
#3215 = EDGE_LOOP ( 'NONE', ( #8526, #5947, #6571, #6313 ) ) ;
#3216 = DIRECTION ( 'NONE',  ( 1.000000000000000000, 0.000000000000000000, 0.000000000000000000 ) ) ;
#3217 = VERTEX_POINT ( 'NONE', #3578 ) ;
#3218 = ORIENTED_EDGE ( 'NONE', *, *, #4035, .F. ) ;
#3219 = DIRECTION ( 'NONE',  ( 0.000000000000000000, 0.000000000000000000, 1.000000000000000000 ) ) ;
#3220 = ORIENTED_EDGE ( 'NONE', *, *, #2132, .T. ) ;
#3221 = ADVANCED_BREP_SHAPE_REPRESENTATION ( '', ( #2963, #7563 ), #2705 ) ;
#3222 = FACE_BOUND ( 'NONE', #6447, .T. ) ;
#3223 = CARTESIAN_POINT ( 'NONE',  ( 0.000000000000000000, -294.9999999999998295, -2.775557561562891351E-14 ) ) ;
#3224 =( LENGTH_UNIT ( ) NAMED_UNIT ( * ) SI_UNIT ( .MILLI., .METRE. ) );
#3225 = ADVANCED_FACE ( 'NONE', ( #4223 ), #8183, .F. ) ;
#3226 = ORIENTED_EDGE ( 'NONE', *, *, #623, .T. ) ;
#3227 = CARTESIAN_POINT ( 'NONE',  ( 0.000000000000000000, -299.9999999999999432, -2.775557561562891351E-14 ) ) ;
#3228 = ITEM_DEFINED_TRANSFORMATION ( 'NONE', 'NONE', #7023,  #7563 ) ;
#3229 =( REPRESENTATION_RELATIONSHIP ('NONE','NONE', #1279, #83 ) REPRESENTATION_RELATIONSHIP_WITH_TRANSFORMATION ( #6373 )SHAPE_REPRESENTATION_RELATIONSHIP( ) );
#3230 = EDGE_CURVE ( 'NONE', #6497, #2216, #2183, .T. ) ;
#3231 = ORIENTED_EDGE ( 'NONE', *, *, #6487, .F. ) ;
#3232 = FACE_OUTER_BOUND ( 'NONE', #4254, .T. ) ;
#3233 = AXIS2_PLACEMENT_3D ( 'NONE', #6716, #31, #660 ) ;
#3234 = VECTOR ( 'NONE', #1595, 1000.000000000000000 ) ;
#3235 = VERTEX_POINT ( 'NONE', #5404 ) ;
#3236 = CARTESIAN_POINT ( 'NONE',  ( -3.660532965668689354, 7.124194613927617326, 4.229404912230172453E-14 ) ) ;
#3237 = VERTEX_POINT ( 'NONE', #1440 ) ;
#3238 = CYLINDRICAL_SURFACE ( 'NONE', #6588, 8.000000000000000000 ) ;
#3239 = APPLICATION_CONTEXT ( 'automotive_design' ) ;
#3240 = PRODUCT_DEFINITION_CONTEXT ( 'detailed design', #1030, 'design' ) ;
#3241 = AXIS2_PLACEMENT_3D ( 'NONE', #6891, #8318, #2340 ) ;
#3242 = EDGE_CURVE ( 'NONE', #6699, #3472, #2533, .T. ) ;
#3243 = CARTESIAN_POINT ( 'NONE',  ( -5.080504117408896292, -2.106769544347821377, -8.401000000000047763 ) ) ;
#3244 = ADVANCED_FACE ( 'NONE', ( #8054, #2368, #3027 ), #2097, .T. ) ;
#3245 = CYLINDRICAL_SURFACE ( 'NONE', #4195, 5.500000000000000000 ) ;
#3246 = CARTESIAN_POINT ( 'NONE',  ( 0.000000000000000000, 0.000000000000000000, 0.000000000000000000 ) ) ;
#3247 = AXIS2_PLACEMENT_3D ( 'NONE', #1992, #4560, #3387 ) ;
#3248 = AXIS2_PLACEMENT_3D ( 'NONE', #6840, #6366, #2213 ) ;
#3249 = CARTESIAN_POINT ( 'NONE',  ( 4.681481898396449459, -6.534749472788188740, 1.717715054395940744E-13 ) ) ;
#3250 = ORIENTED_EDGE ( 'NONE', *, *, #3471, .T. ) ;
#3251 = FILL_AREA_STYLE ('',( #5768 ) ) ;
#3252 = ORIENTED_EDGE ( 'NONE', *, *, #3763, .T. ) ;
#3253 = CARTESIAN_POINT ( 'NONE',  ( 0.000000000000000000, 0.000000000000000000, 0.000000000000000000 ) ) ;
#3254 = EDGE_CURVE ( 'NONE', #1251, #5411, #7780, .T. ) ;
#3255 = EDGE_CURVE ( 'NONE', #8489, #758, #6169, .T. ) ;
#3256 = ORIENTED_EDGE ( 'NONE', *, *, #2527, .T. ) ;
#3257 = DIRECTION ( 'NONE',  ( 0.000000000000000000, -1.024214141749972931E-29, 1.000000000000000000 ) ) ;
#3258 = ORIENTED_EDGE ( 'NONE', *, *, #6503, .F. ) ;
#3259 = PRODUCT_DEFINITION_FORMATION_WITH_SPECIFIED_SOURCE ( 'ANY', '', #7853, .NOT_KNOWN. ) ;
#3260 = ORIENTED_EDGE ( 'NONE', *, *, #7184, .T. ) ;
#3261 = DIRECTION ( 'NONE',  ( 0.000000000000000000, 1.064348848528640545E-29, -1.000000000000000000 ) ) ;
#3262 = VERTEX_POINT ( 'NONE', #833 ) ;
#3263 = CARTESIAN_POINT ( 'NONE',  ( -6.686525924293513334, 5.377136764700441773, -0.3167204509602711826 ) ) ;
#3264 = ADVANCED_FACE ( 'NONE', ( #7402 ), #3511, .T. ) ;
#3265 = DIRECTION ( 'NONE',  ( 1.000000000000000000, -1.284024588418159550E-35, 3.851859888774464864E-33 ) ) ;
#3266 = CARTESIAN_POINT ( 'NONE',  ( 0.000000000000000000, 0.000000000000000000, 0.000000000000000000 ) ) ;
#3267 = DIRECTION ( 'NONE',  ( -0.000000000000000000, -0.000000000000000000, 1.000000000000000000 ) ) ;
#3268 = ORIENTED_EDGE ( 'NONE', *, *, #6617, .F. ) ;
#3269 = AXIS2_PLACEMENT_3D ( 'NONE', #3787, #5733, #7019 ) ;
#3270 = FACE_OUTER_BOUND ( 'NONE', #8065, .T. ) ;
#3271 = PRODUCT ( 'Flipper', 'Flipper', '', ( #5996 ) ) ;
#3272 = EDGE_CURVE ( 'NONE', #2069, #5906, #6962, .T. ) ;
#3273 = AXIS2_PLACEMENT_3D ( 'NONE', #8484, #1125, #6444 ) ;
#3274 = ORIENTED_EDGE ( 'NONE', *, *, #4440, .F. ) ;
#3275 = CARTESIAN_POINT ( 'NONE',  ( 10.00000000000000888, -650.0000000000002274, -1.110223024625156540E-13 ) ) ;
#3276 = EDGE_LOOP ( 'NONE', ( #4309, #7256, #3094, #7788 ) ) ;
#3277 = CARTESIAN_POINT ( 'NONE',  ( 8.000000000000007105, 4.618802153517065356, -7.685468820183672278 ) ) ;
#3278 = ORIENTED_EDGE ( 'NONE', *, *, #943, .T. ) ;
#3279 = DIRECTION ( 'NONE',  ( -1.000000000000000000, 3.549874073494553124E-30, 0.000000000000000000 ) ) ;
#3280 = EDGE_CURVE ( 'NONE', #4655, #3844, #2392, .T. ) ;
#3281 = CARTESIAN_POINT ( 'NONE',  ( 0.000000000000000000, 0.000000000000000000, 18.00000000000000355 ) ) ;
#3282 = FACE_OUTER_BOUND ( 'NONE', #2142, .T. ) ;
#3283 = LINE ( 'NONE', #4604, #8475 ) ;
#3284 = CARTESIAN_POINT ( 'NONE',  ( 50.00000000000004263, -425.0000000000000000, 25.00000000000000355 ) ) ;
#3285 = CARTESIAN_POINT ( 'NONE',  ( -4.000000000000003553, -6.928203230275431501, 0.000000000000000000 ) ) ;
#3286 = VERTEX_POINT ( 'NONE', #2147 ) ;
#3287 = VECTOR ( 'NONE', #2892, 1000.000000000000000 ) ;
#3288 = CARTESIAN_POINT ( 'NONE',  ( -49.99999999999953815, 120.0000000000003268, 9.999999999999980460 ) ) ;
#3289 = VERTEX_POINT ( 'NONE', #6805 ) ;
#3290 = LINE ( 'NONE', #2645, #5576 ) ;
#3291 = EDGE_CURVE ( 'NONE', #3910, #363, #6042, .T. ) ;
#3292 = EDGE_CURVE ( 'NONE', #7541, #5649, #2219, .T. ) ;
#3293 = CIRCLE ( 'NONE', #8170, 75.00000000000000000 ) ;
#3294 = DIRECTION ( 'NONE',  ( 0.000000000000000000, -0.4999999999999987232, 0.8660254037844393737 ) ) ;
#3295 = CARTESIAN_POINT ( 'NONE',  ( 0.000000000000000000, 0.000000000000000000, 0.000000000000000000 ) ) ;
#3296 = CARTESIAN_POINT ( 'NONE',  ( -4.391120273202897044E-30, -294.9999999999998295, 75.00000000000000000 ) ) ;
#3297 = CONTEXT_DEPENDENT_SHAPE_REPRESENTATION ( #4623, #3481 ) ;
#3298 = CARTESIAN_POINT ( 'NONE',  ( 0.000000000000000000, 0.000000000000000000, 0.000000000000000000 ) ) ;
#3299 = CARTESIAN_POINT ( 'NONE',  ( 275.0000000000000000, -425.0000000000000000, 75.00000000000000000 ) ) ;
#3300 = VERTEX_POINT ( 'NONE', #211 ) ;
#3301 = DIRECTION ( 'NONE',  ( 1.000000000000000000, 2.775557561562914622E-15, 0.000000000000000000 ) ) ;
#3302 = ORIENTED_EDGE ( 'NONE', *, *, #4618, .T. ) ;
#3303 = EDGE_CURVE ( 'NONE', #5371, #7390, #3422, .T. ) ;
#3304 = LINE ( 'NONE', #24, #7814 ) ;
#3305 = ORIENTED_EDGE ( 'NONE', *, *, #854, .T. ) ;
#3306 = DIRECTION ( 'NONE',  ( -7.703719777548943412E-34, 0.000000000000000000, 1.000000000000000000 ) ) ;
#3307 = DIRECTION ( 'NONE',  ( 0.000000000000000000, -4.930380657631321594E-32, -1.000000000000000000 ) ) ;
#3308 = EDGE_CURVE ( 'NONE', #530, #7908, #3070, .T. ) ;
#3309 = FACE_OUTER_BOUND ( 'NONE', #3784, .T. ) ;
#3310 = CARTESIAN_POINT ( 'NONE',  ( 50.00000000000004263, 500.0000000000000000, 50.00000000000000000 ) ) ;
#3311 = DIRECTION ( 'NONE',  ( 0.000000000000000000, 0.000000000000000000, -1.000000000000000000 ) ) ;
#3312 = ORIENTED_EDGE ( 'NONE', *, *, #445, .F. ) ;
#3313 = CARTESIAN_POINT ( 'NONE',  ( 8.000000000000117240, -1.110223024625156540E-13, -8.400000000000018119 ) ) ;
#3314 = APPLICATION_PROTOCOL_DEFINITION ( 'draft international standard', 'automotive_design', 1998, #7856 ) ;
#3315 = CYLINDRICAL_SURFACE ( 'NONE', #4133, 39.75000000000007105 ) ;
#3316 = DIRECTION ( 'NONE',  ( 3.549874073494553124E-30, -0.5000000000000009992, -0.8660254037844380415 ) ) ;
#3317 = ORIENTED_EDGE ( 'NONE', *, *, #8370, .T. ) ;
#3318 = CIRCLE ( 'NONE', #5723, 75.00000000000005684 ) ;
#3319 = FACE_OUTER_BOUND ( 'NONE', #5588, .T. ) ;
#3320 = CARTESIAN_POINT ( 'NONE',  ( 0.000000000000000000, 0.000000000000000000, -45.00000000000000711 ) ) ;
#3321 = ORIENTED_EDGE ( 'NONE', *, *, #2226, .T. ) ;
#3322 = CARTESIAN_POINT ( 'NONE',  ( 6.689127551061982757, 5.375634714784596646, -8.082649155111388595 ) ) ;
#3323 = ORIENTED_EDGE ( 'NONE', *, *, #6119, .F. ) ;
#3324 = CARTESIAN_POINT ( 'NONE',  ( -34.92499999999998295, 6.809036203259282560E-16, -5.559999999999998721 ) ) ;
#3325 = AXIS2_PLACEMENT_3D ( 'NONE', #4241, #227, #2884 ) ;
#3326 = AXIS2_PLACEMENT_3D ( 'NONE', #2552, #7861, #2462 ) ;
#3327 = CARTESIAN_POINT ( 'NONE',  ( 0.000000000000000000, 299.9999999999999432, -6.938893903907228378E-14 ) ) ;
#3328 = PLANE ( 'NONE',  #8306 ) ;
#3330 = FACE_OUTER_BOUND ( 'NONE', #3585, .T. ) ;
#3329 = VECTOR ( 'NONE', #4417, 1000.000000000000000 ) ;
#3331 = CIRCLE ( 'NONE', #3209, 5.400000000000034994 ) ;
#3332 = CARTESIAN_POINT ( 'NONE',  ( -31.74999999999994316, -2.397948410737325939E-28, 8.000000000000000000 ) ) ;
#3333 = CARTESIAN_POINT ( 'NONE',  ( 0.000000000000000000, -299.9999999999999432, 24.49999999999996803 ) ) ;
#3334 = ADVANCED_FACE ( 'NONE', ( #5201 ), #2588, .T. ) ;
#3335 = LINE ( 'NONE', #1286, #356 ) ;
#3336 = DIRECTION ( 'NONE',  ( 0.000000000000000000, 0.000000000000000000, 1.000000000000000000 ) ) ;
#3337 = ORIENTED_EDGE ( 'NONE', *, *, #7927, .F. ) ;
#3338 = CARTESIAN_POINT ( 'NONE',  ( -275.0000000000000000, -425.0000000000000000, -75.00000000000000000 ) ) ;
#3339 = EDGE_LOOP ( 'NONE', ( #7406, #4421, #1814 ) ) ;
#3340 = CARTESIAN_POINT ( 'NONE',  ( 0.000000000000000000, 1.224646799147353454E-15, -10.00000000000000178 ) ) ;
#3341 = SURFACE_STYLE_USAGE ( .BOTH. , #7960 ) ;
#3342 = CONICAL_SURFACE ( 'NONE', #4322, 8.000000000000007105, 1.047197551196597631 ) ;
#3343 = FACE_OUTER_BOUND ( 'NONE', #3806, .T. ) ;
#3344 = CARTESIAN_POINT ( 'NONE',  ( -2.309976723937749110, 7.903938623646892481, -8.269346954796169769 ) ) ;
#3345 = AXIS2_PLACEMENT_3D ( 'NONE', #4343, #3815, #7011 ) ;
#3346 = EDGE_CURVE ( 'NONE', #2011, #2131, #1840, .T. ) ;
#3347 = DIRECTION ( 'NONE',  ( 3.919652622816902408E-30, 3.944304526105059027E-30, -1.000000000000000000 ) ) ;
#3348 = VERTEX_POINT ( 'NONE', #3771 ) ;
#3349 = FACE_OUTER_BOUND ( 'NONE', #1586, .T. ) ;
#3350 = EDGE_LOOP ( 'NONE', ( #3026, #3682, #5381, #264 ) ) ;
#3351 = CYLINDRICAL_SURFACE ( 'NONE', #1835, 10.49999999999999645 ) ;
#3352 = DIRECTION ( 'NONE',  ( 0.000000000000000000, 0.000000000000000000, 1.000000000000000000 ) ) ;
#3353 = CARTESIAN_POINT ( 'NONE',  ( 8.000000000000008882, 1.572549600175327855, -0.06894455525510422012 ) ) ;
#3354 = CARTESIAN_POINT ( 'NONE',  ( -8.000000000000000000, -3.867591403079186030, -7.902324684675432920 ) ) ;
#3355 = EDGE_LOOP ( 'NONE', ( #1838, #1478 ) ) ;
#3356 = EDGE_CURVE ( 'NONE', #5078, #6377, #5904, .T. ) ;
#3357 = ORIENTED_EDGE ( 'NONE', *, *, #4058, .F. ) ;
#3358 = SHAPE_DEFINITION_REPRESENTATION ( #7238, #6122 ) ;
#3359 = DIRECTION ( 'NONE',  ( 1.774937036747276562E-30, 1.000000000000000000, -1.224646799147299959E-16 ) ) ;
#3360 = CARTESIAN_POINT ( 'NONE',  ( 5.000000000000004441, -2.342598717236951789, 4.057500000000047180 ) ) ;
#3361 = EDGE_CURVE ( 'NONE', #4294, #2221, #5172, .T. ) ;
#3362 = VECTOR ( 'NONE', #6554, 1000.000000000000000 ) ;
#3363 = DIRECTION ( 'NONE',  ( -0.5000000000000042188, 1.060575238724958684E-16, -0.8660254037844361541 ) ) ;
#3364 = EDGE_LOOP ( 'NONE', ( #2845, #7746, #8182, #1866 ) ) ;
#3365 = DIRECTION ( 'NONE',  ( 3.498359009886546906E-15, 1.000000000000000000, -3.747089299799789961E-30 ) ) ;
#3366 = DIRECTION ( 'NONE',  ( 0.000000000000000000, 0.000000000000000000, 1.000000000000000000 ) ) ;
#3367 = ORIENTED_EDGE ( 'NONE', *, *, #5113, .T. ) ;
#3368 = AXIS2_PLACEMENT_3D ( 'NONE', #6435, #7127, #8436 ) ;
#3369 = DIRECTION ( 'NONE',  ( 0.000000000000000000, -0.000000000000000000, 1.000000000000000000 ) ) ;
#3370 = VERTEX_POINT ( 'NONE', #5245 ) ;
#3371 = DIRECTION ( 'NONE',  ( -3.919652622816902408E-30, -3.944304526105059027E-30, 1.000000000000000000 ) ) ;
#3372 = VECTOR ( 'NONE', #619, 1000.000000000000000 ) ;
#3373 = CARTESIAN_POINT ( 'NONE',  ( 9.999999999999896971, 0.000000000000000000, 79.99999999999995737 ) ) ;
#3374 = CARTESIAN_POINT ( 'NONE',  ( -8.000000000000229150, 4.618802153516954334, -0.7145311798163467287 ) ) ;
#3375 = VECTOR ( 'NONE', #7753, 1000.000000000000000 ) ;
#3376 = CARTESIAN_POINT ( 'NONE',  ( 0.000000000000000000, 0.000000000000000000, 0.000000000000000000 ) ) ;
#3377 = CARTESIAN_POINT ( 'NONE',  ( 8.000000000000007105, 4.618802153516732290, -7.685468820183672278 ) ) ;
#3378 = CARTESIAN_POINT ( 'NONE',  ( 8.000000000000007105, -4.618802153517121312, -0.7145311798163467287 ) ) ;
#3379 = CARTESIAN_POINT ( 'NONE',  ( 0.000000000000000000, -1.759474945355374631, 3.047500000000091802 ) ) ;
#3380 = VERTEX_POINT ( 'NONE', #5799 ) ;
#3381 = CIRCLE ( 'NONE', #2139, 75.00000000000005684 ) ;
#3382 = CARTESIAN_POINT ( 'NONE',  ( -7.999999999999894307, 3.115336682266907964, -0.3193931313914263881 ) ) ;
#3383 = LINE ( 'NONE', #151, #7105 ) ;
#3384 = FACE_OUTER_BOUND ( 'NONE', #8499, .T. ) ;
#3385 = DIRECTION ( 'NONE',  ( 0.000000000000000000, -4.930380657631321594E-32, -1.000000000000000000 ) ) ;
#3386 = CIRCLE ( 'NONE', #1153, 25.00000000000000711 ) ;
#3387 = DIRECTION ( 'NONE',  ( 0.000000000000000000, -0.000000000000000000, 1.000000000000000000 ) ) ;
#3388 = ADVANCED_FACE ( 'NONE', ( #7246 ), #6548, .F. ) ;
#3389 = PRODUCT_RELATED_PRODUCT_CATEGORY ( 'part', '', ( #5800 ) ) ;
#3390 = AXIS2_PLACEMENT_3D ( 'NONE', #2878, #5510, #4184 ) ;
#3391 = CARTESIAN_POINT ( 'NONE',  ( 10.00000000000000888, -650.0000000000002274, -1.110223024625156540E-13 ) ) ;
#3392 = CIRCLE ( 'NONE', #3248, 8.000000000000001776 ) ;
#3393 = CYLINDRICAL_SURFACE ( 'NONE', #2626, 5.749999999999984013 ) ;
#3394 = CARTESIAN_POINT ( 'NONE',  ( 8.000000000000007105, 4.618802153516899267, -7.685468820183672278 ) ) ;
#3395 = DIRECTION ( 'NONE',  ( 0.000000000000000000, -0.5000000000000009992, -0.8660254037844380415 ) ) ;
#3396 = ORIENTED_EDGE ( 'NONE', *, *, #7943, .T. ) ;
#3397 =( GEOMETRIC_REPRESENTATION_CONTEXT ( 3 ) GLOBAL_UNCERTAINTY_ASSIGNED_CONTEXT ( ( #1152 ) ) GLOBAL_UNIT_ASSIGNED_CONTEXT ( ( #5243, #669, #6048 ) ) REPRESENTATION_CONTEXT ( 'NONE', 'WORKASPACE' ) );
#3398 = CARTESIAN_POINT ( 'NONE',  ( -7.999999999999888978, -1.555946510856243581, -8.332911297836714581 ) ) ;
#3399 = ORIENTED_EDGE ( 'NONE', *, *, #3887, .F. ) ;
#3400 = CARTESIAN_POINT ( 'NONE',  ( -50.00000000000004263, -500.0000000000000000, 50.00000000000000000 ) ) ;
#3401 = EDGE_CURVE ( 'NONE', #6357, #1987, #5106, .T. ) ;
#3402 = CARTESIAN_POINT ( 'NONE',  ( -3.319543390096229452, 7.321065037175419121, -0.01688885742780804958 ) ) ;
#3403 = CARTESIAN_POINT ( 'NONE',  ( 8.000000000000012434, 0.7809653281572527250, 1.900487823754473040E-14 ) ) ;
#3404 = FACE_OUTER_BOUND ( 'NONE', #1082, .T. ) ;
#3405 =( REPRESENTATION_RELATIONSHIP ('NONE','NONE', #1279, #4003 ) REPRESENTATION_RELATIONSHIP_WITH_TRANSFORMATION ( #5899 )SHAPE_REPRESENTATION_RELATIONSHIP( ) );
#3406 = PLANE ( 'NONE',  #3233 ) ;
#3407 = EDGE_LOOP ( 'NONE', ( #2715, #3758, #5527 ) ) ;
#3408 = PRODUCT_DEFINITION_FORMATION_WITH_SPECIFIED_SOURCE ( 'ANY', '', #3271, .NOT_KNOWN. ) ;
#3409 = VERTEX_POINT ( 'NONE', #5755 ) ;
#3410 = EDGE_CURVE ( 'NONE', #1795, #1251, #6138, .T. ) ;
#3411 = DIRECTION ( 'NONE',  ( 1.000000000000000000, 0.000000000000000000, 0.000000000000000000 ) ) ;
#3412 = CARTESIAN_POINT ( 'NONE',  ( -99.99999999999972999, 0.000000000000000000, -2.775557561562891351E-14 ) ) ;
#3413 = VERTEX_POINT ( 'NONE', #1934 ) ;
#3414 = DIRECTION ( 'NONE',  ( 0.000000000000000000, 0.000000000000000000, 1.000000000000000000 ) ) ;
#3415 = ORIENTED_EDGE ( 'NONE', *, *, #5482, .T. ) ;
#3416 = PLANE ( 'NONE',  #739 ) ;
#3417 = PRODUCT_DEFINITION_SHAPE ( 'NONE', 'NONE',  #8615 ) ;
#3418 = ORIENTED_EDGE ( 'NONE', *, *, #6718, .F. ) ;
#3419 = PLANE ( 'NONE',  #897 ) ;
#3420 = EDGE_CURVE ( 'NONE', #8418, #6851, #3888, .T. ) ;
#3421 = DIRECTION ( 'NONE',  ( 0.000000000000000000, 0.000000000000000000, 1.000000000000000000 ) ) ;
#3422 = B_SPLINE_CURVE_WITH_KNOTS ( 'NONE', 3,
 ( #2871, #4877, #1560, #6888, #917, #4596 ),
 .UNSPECIFIED., .F., .F.,
 ( 4, 2, 4 ),
 ( 0.01291313371729486958, 0.01525081363757331207, 0.01758849355785175456 ),
 .UNSPECIFIED. ) ;
#3423 = CARTESIAN_POINT ( 'NONE',  ( 5.000000000000115463, -14.99999999999990230, -20.00000000000001776 ) ) ;
#3424 = VERTEX_POINT ( 'NONE', #1756 ) ;
#3425 = DIRECTION ( 'NONE',  ( 1.000000000000000000, 8.881784197001244435E-16, 0.000000000000000000 ) ) ;
#3426 = DIRECTION ( 'NONE',  ( 3.646298014371739284E-59, 1.027162637006519249E-29, -1.000000000000000000 ) ) ;
#3427 = CARTESIAN_POINT ( 'NONE',  ( -3.318518101603116666, -7.321656987762883873, -8.399999999999991473 ) ) ;
#3428 = DIRECTION ( 'NONE',  ( 0.000000000000000000, 0.000000000000000000, -1.000000000000000000 ) ) ;
#3429 = ORIENTED_EDGE ( 'NONE', *, *, #144, .F. ) ;
#3430 = EDGE_CURVE ( 'NONE', #484, #4252, #7078, .T. ) ;
#3431 = SURFACE_STYLE_FILL_AREA ( #4037 ) ;
#3432 = ORIENTED_EDGE ( 'NONE', *, *, #1381, .T. ) ;
#3433 = CONICAL_SURFACE ( 'NONE', #4539, 8.000000000000007105, 1.047197551196597631 ) ;
#3434 = UNCERTAINTY_MEASURE_WITH_UNIT (LENGTH_MEASURE( 1.000000000000000082E-05 ), #1265, 'distance_accuracy_value', 'NONE');
#3435 = AXIS2_PLACEMENT_3D ( 'NONE', #7386, #2244, #4122 ) ;
#3436 = CARTESIAN_POINT ( 'NONE',  ( 7.345652830558639046, -4.996589667937789692, -7.903584543331145795 ) ) ;
#3437 = CARTESIAN_POINT ( 'NONE',  ( 3.999999999999559464, 6.928203230274987412, -8.400000000000018119 ) ) ;
#3438 = CONTEXT_DEPENDENT_SHAPE_REPRESENTATION ( #5351, #436 ) ;
#3439 = CARTESIAN_POINT ( 'NONE',  ( 5.080504117408890075, 2.106769544347818268, -8.400000000000018119 ) ) ;
#3440 = DIRECTION ( 'NONE',  ( 1.000000000000000000, -0.000000000000000000, -6.938893903907228378E-17 ) ) ;
#3441 = ORIENTED_EDGE ( 'NONE', *, *, #5342, .F. ) ;
#3442 = COLOUR_RGB ( '',0.7921568627450980005, 0.8196078431372548767, 0.9333333333333333481 ) ;
#3443 = CARTESIAN_POINT ( 'NONE',  ( 2.220446049250313081E-13, 9.237604307034075646, 0.000000000000000000 ) ) ;
#3444 = EDGE_LOOP ( 'NONE', ( #4635, #1953 ) ) ;
#3445 = DIRECTION ( 'NONE',  ( 0.000000000000000000, -1.000000000000000000, -1.224646799147352714E-16 ) ) ;
#3446 = DIRECTION ( 'NONE',  ( -0.000000000000000000, -0.000000000000000000, 1.000000000000000000 ) ) ;
#3447 =( NAMED_UNIT ( * ) PLANE_ANGLE_UNIT ( ) SI_UNIT ( $, .RADIAN. ) );
#3448 = CARTESIAN_POINT ( 'NONE',  ( 44.99999999999992895, -425.0000000000000000, -3.122502256758253953E-15 ) ) ;
#3449 = AXIS2_PLACEMENT_3D ( 'NONE', #1629, #75, #3486 ) ;
#3450 = EDGE_LOOP ( 'NONE', ( #7509, #5011, #8124, #6187 ) ) ;
#3451 = LINE ( 'NONE', #5321, #7277 ) ;
#3452 = ORIENTED_EDGE ( 'NONE', *, *, #2653, .T. ) ;
#3453 = VERTEX_POINT ( 'NONE', #8463 ) ;
#3454 = EDGE_CURVE ( 'NONE', #3046, #3235, #924, .T. ) ;
#3455 = SHAPE_REPRESENTATION ( 'hex nut style 1_am_B18.2.4.1M - Hex nut, Style 1,  M10 x 1.5, with 16mm WAF --D-N', ( #7563 ), #7435 ) ;
#3456 = CYLINDRICAL_SURFACE ( 'NONE', #7055, 10.00000000000000178 ) ;
#3457 = VECTOR ( 'NONE', #256, 1000.000000000000000 ) ;
#3458 = CARTESIAN_POINT ( 'NONE',  ( -5.499999999999999112, 60.00000000000000000, -50.00000000000000000 ) ) ;
#3459 = ORIENTED_EDGE ( 'NONE', *, *, #6854, .T. ) ;
#3460 = CARTESIAN_POINT ( 'NONE',  ( -17.49999999999958078, 120.0000000000003268, 0.000000000000000000 ) ) ;
#3461 = EDGE_CURVE ( 'NONE', #863, #7532, #8509, .T. ) ;
#3462 = CARTESIAN_POINT ( 'NONE',  ( 350.0000000000000568, 59.99999999999988631, -50.00000000000001421 ) ) ;
#3463 = ORIENTED_EDGE ( 'NONE', *, *, #8095, .F. ) ;
#3464 = EDGE_LOOP ( 'NONE', ( #4377, #7954, #2106, #4854, #4969, #5551 ) ) ;
#3465 = CARTESIAN_POINT ( 'NONE',  ( 0.000000000000000000, 0.000000000000000000, 0.000000000000000000 ) ) ;
#3466 = CARTESIAN_POINT ( 'NONE',  ( 8.000000000000007105, 4.618802153516732290, -8.400000000000018119 ) ) ;
#3467 = CIRCLE ( 'NONE', #4019, 5.500000000000023981 ) ;
#3468 = ORIENTED_EDGE ( 'NONE', *, *, #6930, .T. ) ;
#3469 = CARTESIAN_POINT ( 'NONE',  ( 5.000000000000115463, 7.027796151710889561, -4.057500000000047180 ) ) ;
#3470 = CARTESIAN_POINT ( 'NONE',  ( 1.110223024625156540E-13, 9.237604307033992157, -0.7145311798163467287 ) ) ;
#3471 = EDGE_CURVE ( 'NONE', #5176, #3689, #2501, .T. ) ;
#3472 = VERTEX_POINT ( 'NONE', #7162 ) ;
#3473 = VECTOR ( 'NONE', #2593, 1000.000000000000000 ) ;
#3474 = CARTESIAN_POINT ( 'NONE',  ( 10.00000000000000888, -650.0000000000002274, -1.110223024625156540E-13 ) ) ;
#3475 = DIRECTION ( 'NONE',  ( -3.549874073494553124E-30, 1.000000000000000000, -1.478898702612462838E-15 ) ) ;
#3476 = AXIS2_PLACEMENT_3D ( 'NONE', #5700, #1830, #497 ) ;
#3477 = CARTESIAN_POINT ( 'NONE',  ( 275.0000000000000000, 425.0000000000000000, 1.561424668912875158E-13 ) ) ;
#3478 = LINE ( 'NONE', #1390, #4927 ) ;
#3479 = ORIENTED_EDGE ( 'NONE', *, *, #8209, .F. ) ;
#3480 = AXIS2_PLACEMENT_3D ( 'NONE', #6864, #7636, #5517 ) ;
#3481 = PRODUCT_DEFINITION_SHAPE ( 'NONE', 'NONE',  #8631 ) ;
#3482 = DIRECTION ( 'NONE',  ( -1.000000000000000000, -8.881784197001244435E-16, 0.000000000000000000 ) ) ;
#3483 = ORIENTED_EDGE ( 'NONE', *, *, #5225, .T. ) ;
#3484 = ADVANCED_FACE ( 'NONE', ( #3845 ), #2631, .T. ) ;
#3485 = CARTESIAN_POINT ( 'NONE',  ( 5.000000000000115463, -14.99999999999990230, 0.000000000000000000 ) ) ;
#3486 = DIRECTION ( 'NONE',  ( 1.000000000000000000, 2.715219353702835081E-15, -3.821045009664285041E-30 ) ) ;
#3487 = EDGE_CURVE ( 'NONE', #363, #6830, #6311, .T. ) ;
#3488 = CYLINDRICAL_SURFACE ( 'NONE', #7567, 4.250000000000003553 ) ;
#3489 = VERTEX_POINT ( 'NONE', #2068 ) ;
#3490 = DIRECTION ( 'NONE',  ( -1.000000000000000000, 3.549874073494553124E-30, 0.000000000000000000 ) ) ;
#3491 = ORIENTED_EDGE ( 'NONE', *, *, #4136, .T. ) ;
#3492 = EDGE_LOOP ( 'NONE', ( #2266, #4191, #6871, #1910, #3901, #1335 ) ) ;
#3493 = AXIS2_PLACEMENT_3D ( 'NONE', #1988, #6749, #7955 ) ;
#3494 = B_SPLINE_CURVE_WITH_KNOTS ( 'NONE', 3,
 ( #3378, #6061, #97, #5479, #4734, #193 ),
 .UNSPECIFIED., .F., .F.,
 ( 4, 2, 4 ),
 ( 0.008240550023493491139, 0.01057684187039397566, 0.01291313371729446019 ),
 .UNSPECIFIED. ) ;
#3495 = FACE_OUTER_BOUND ( 'NONE', #4760, .T. ) ;
#3496 = CARTESIAN_POINT ( 'NONE',  ( 44.99999999999992895, 425.0000000000000000, 25.00000000000000355 ) ) ;
#3497 = ADVANCED_FACE ( 'NONE', ( #4725, #4685 ), #5291, .F. ) ;
#3498 = ORIENTED_EDGE ( 'NONE', *, *, #529, .T. ) ;
#3499 = DIRECTION ( 'NONE',  ( 1.000000000000000000, -0.000000000000000000, -6.938893903907228378E-17 ) ) ;
#3500 = PLANE ( 'NONE',  #6268 ) ;
#3501 = CARTESIAN_POINT ( 'NONE',  ( -468.9721151762510090, 37.40135105920447245, 82.00000000000000000 ) ) ;
#3502 = ORIENTED_EDGE ( 'NONE', *, *, #745, .F. ) ;
#3503 = ORIENTED_EDGE ( 'NONE', *, *, #623, .F. ) ;
#3504 = CARTESIAN_POINT ( 'NONE',  ( 0.7999999999999674039, -1.387778780781445676E-14, 0.000000000000000000 ) ) ;
#3505 = EDGE_CURVE ( 'NONE', #6381, #5371, #5611, .T. ) ;
#3506 = CARTESIAN_POINT ( 'NONE',  ( 0.000000000000000000, 0.000000000000000000, 0.000000000000000000 ) ) ;
#3507 = EDGE_LOOP ( 'NONE', ( #977, #7262, #4281 ) ) ;
#3508 = AXIS2_PLACEMENT_3D ( 'NONE', #1850, #4391, #3778 ) ;
#3509 = CARTESIAN_POINT ( 'NONE',  ( 0.000000000000000000, 0.000000000000000000, 0.000000000000000000 ) ) ;
#3510 = DIRECTION ( 'NONE',  ( 0.000000000000000000, 1.000000000000000000, 1.795949010423047620E-16 ) ) ;
#3511 = CONICAL_SURFACE ( 'NONE', #5330, 8.000000000000007105, 1.047197551196597631 ) ;
#3512 = DIRECTION ( 'NONE',  ( 1.000000000000000000, 0.000000000000000000, 0.000000000000000000 ) ) ;
#3513 = ORIENTED_EDGE ( 'NONE', *, *, #4938, .T. ) ;
#3514 = ORIENTED_EDGE ( 'NONE', *, *, #4352, .F. ) ;
#3515 = AXIS2_PLACEMENT_3D ( 'NONE', #3376, #2075, #3896 ) ;
#3516 = EDGE_CURVE ( 'NONE', #4229, #1438, #461, .T. ) ;
#3517 = CARTESIAN_POINT ( 'NONE',  ( 0.000000000000000000, 0.000000000000000000, 10.00000000000000888 ) ) ;
#3518 = AXIS2_PLACEMENT_3D ( 'NONE', #5869, #2534, #5826 ) ;
#3519 = DIRECTION ( 'NONE',  ( 0.000000000000000000, 0.000000000000000000, -1.000000000000000000 ) ) ;
#3520 = FACE_OUTER_BOUND ( 'NONE', #6625, .T. ) ;
#3521 = CARTESIAN_POINT ( 'NONE',  ( -6.689127551061946342, -5.375634714785059387, -8.082649155111232275 ) ) ;
#3522 = FACE_BOUND ( 'NONE', #3597, .T. ) ;
#3523 = ORIENTED_EDGE ( 'NONE', *, *, #4224, .F. ) ;
#3524 = DIRECTION ( 'NONE',  ( 1.000000000000000000, 0.000000000000000000, 0.000000000000000000 ) ) ;
#3525 = ORIENTED_EDGE ( 'NONE', *, *, #6695, .F. ) ;
#3526 = AXIS2_PLACEMENT_3D ( 'NONE', #6869, #3554, #234 ) ;
#3527 = CARTESIAN_POINT ( 'NONE',  ( 8.572527594031484037E-15, 299.9999999999999432, 70.00000000000001421 ) ) ;
#3528 = AXIS2_PLACEMENT_3D ( 'NONE', #2800, #220, #8156 ) ;
#3529 =( GEOMETRIC_REPRESENTATION_CONTEXT ( 3 ) GLOBAL_UNCERTAINTY_ASSIGNED_CONTEXT ( ( #4657 ) ) GLOBAL_UNIT_ASSIGNED_CONTEXT ( ( #5392, #4735, #1503 ) ) REPRESENTATION_CONTEXT ( 'NONE', 'WORKASPACE' ) );
#3530 = ADVANCED_FACE ( 'NONE', ( #674 ), #2964, .T. ) ;
#3531 =( REPRESENTATION_RELATIONSHIP ('NONE','NONE', #1279, #5506 ) REPRESENTATION_RELATIONSHIP_WITH_TRANSFORMATION ( #554 )SHAPE_REPRESENTATION_RELATIONSHIP( ) );
#3532 = CARTESIAN_POINT ( 'NONE',  ( 5.500000000000000000, 0.000000000000000000, 45.00000000000000000 ) ) ;
#3533 = CARTESIAN_POINT ( 'NONE',  ( 5.000000000000115463, -14.99999999999990230, -20.00000000000001776 ) ) ;
#3534 = EDGE_LOOP ( 'NONE', ( #2223, #3085, #2899 ) ) ;
#3535 = PLANE ( 'NONE',  #3601 ) ;
#3536 = ORIENTED_EDGE ( 'NONE', *, *, #39, .F. ) ;
#3537 = ORIENTED_EDGE ( 'NONE', *, *, #6441, .T. ) ;
#3538 = CIRCLE ( 'NONE', #8401, 5.500000000000023981 ) ;
#3539 = ADVANCED_FACE ( 'NONE', ( #4644 ), #7293, .F. ) ;
#3540 = CARTESIAN_POINT ( 'NONE',  ( 4.000000000000003553, 1.759474945355374409, 3.047499999999869758 ) ) ;
#3541 = EDGE_CURVE ( 'NONE', #4330, #5371, #7136, .T. ) ;
#3542 = PRODUCT_DEFINITION_FORMATION_WITH_SPECIFIED_SOURCE ( 'ANY', '', #3195, .NOT_KNOWN. ) ;
#3543 = FACE_OUTER_BOUND ( 'NONE', #5596, .T. ) ;
#3544 = ORIENTED_EDGE ( 'NONE', *, *, #1926, .T. ) ;
#3545 = DIRECTION ( 'NONE',  ( -1.000000000000000000, 3.549874073494553124E-30, 0.000000000000000000 ) ) ;
#3546 = FACE_OUTER_BOUND ( 'NONE', #7900, .T. ) ;
#3547 = DIRECTION ( 'NONE',  ( 0.9237280213470682178, 0.3830490080632377725, 0.000000000000000000 ) ) ;
#3548 = VERTEX_POINT ( 'NONE', #1325 ) ;
#3549 = EDGE_CURVE ( 'NONE', #1589, #5439, #7366, .T. ) ;
#3550 = ORIENTED_EDGE ( 'NONE', *, *, #6005, .T. ) ;
#3551 = DIRECTION ( 'NONE',  ( -1.463706757734299248E-32, 1.000000000000000000, 5.238529448733281520E-32 ) ) ;
#3552 = ORIENTED_EDGE ( 'NONE', *, *, #3929, .T. ) ;
#3553 = CARTESIAN_POINT ( 'NONE',  ( 0.000000000000000000, 0.000000000000000000, 0.000000000000000000 ) ) ;
#3554 = DIRECTION ( 'NONE',  ( 0.000000000000000000, 0.000000000000000000, 1.000000000000000000 ) ) ;
#3555 = CARTESIAN_POINT ( 'NONE',  ( -5.354491962338311595, 6.146186931204400850, -0.06809871960549450376 ) ) ;
#3556 = ORIENTED_EDGE ( 'NONE', *, *, #1498, .F. ) ;
#3557 = B_SPLINE_CURVE_WITH_KNOTS ( 'NONE', 3,
 ( #7219, #2649, #4700, #7346, #1383, #908, #2209, #5529 ),
 .UNSPECIFIED., .F., .F.,
 ( 4, 2, 2, 4 ),
 ( 0.004673709593152344799, 0.005837709341827777842, 0.007001709090503210886, 0.009329708587854076973 ),
 .UNSPECIFIED. ) ;
#3558 = LINE ( 'NONE', #6185, #1384 ) ;
#3559 = CARTESIAN_POINT ( 'NONE',  ( -8.000000000000229150, 4.440892098500626162E-13, 0.000000000000000000 ) ) ;
#3560 = EDGE_LOOP ( 'NONE', ( #2328, #7849 ) ) ;
#3561 = ADVANCED_FACE ( 'NONE', ( #6734 ), #3416, .F. ) ;
#3562 = ORIENTED_EDGE ( 'NONE', *, *, #452, .T. ) ;
#3563 = ORIENTED_EDGE ( 'NONE', *, *, #6051, .F. ) ;
#3564 = CARTESIAN_POINT ( 'NONE',  ( 0.000000000000000000, 0.000000000000000000, 0.000000000000000000 ) ) ;
#3565 = CIRCLE ( 'NONE', #4679, 4.499999999999997335 ) ;
#3566 = DIRECTION ( 'NONE',  ( -3.498359009886547695E-15, -1.000000000000000000, 3.845696912952415736E-30 ) ) ;
#3567 = CARTESIAN_POINT ( 'NONE',  ( -4.440892098500626162E-13, -9.237604307034018802, -0.7145311798163467287 ) ) ;
#3568 = LINE ( 'NONE', #2711, #7680 ) ;
#3569 = DIRECTION ( 'NONE',  ( -1.000000000000000000, -0.000000000000000000, -0.000000000000000000 ) ) ;
#3570 = EDGE_CURVE ( 'NONE', #569, #2054, #6052, .T. ) ;
#3571 = FACE_BOUND ( 'NONE', #5623, .T. ) ;
#3572 = VERTEX_POINT ( 'NONE', #8036 ) ;
#3573 = EDGE_CURVE ( 'NONE', #4804, #7222, #7823, .T. ) ;
#3574 = CIRCLE ( 'NONE', #8432, 3.309499999999999886 ) ;
#3575 = CARTESIAN_POINT ( 'NONE',  ( 5.000000000000004441, -4.685197434473812095, 0.000000000000000000 ) ) ;
#3576 = ORIENTED_EDGE ( 'NONE', *, *, #222, .T. ) ;
#3577 = ADVANCED_BREP_SHAPE_REPRESENTATION ( '', ( #2946, #7563 ), #1996 ) ;
#3578 = CARTESIAN_POINT ( 'NONE',  ( 0.000000000000000000, 1.759474945355318898, 3.047499999999869758 ) ) ;
#3579 = LINE ( 'NONE', #4227, #8076 ) ;
#3580 = DIRECTION ( 'NONE',  ( -1.463706757734299248E-32, 1.000000000000000000, 5.238529448733281520E-32 ) ) ;
#3581 = AXIS2_PLACEMENT_3D ( 'NONE', #3423, #8256, #6787 ) ;
#3582 = EDGE_LOOP ( 'NONE', ( #1357, #4504 ) ) ;
#3583 = DIRECTION ( 'NONE',  ( -1.000000000000000000, 0.000000000000000000, 0.000000000000000000 ) ) ;
#3584 = ORIENTED_EDGE ( 'NONE', *, *, #6503, .T. ) ;
#3585 = EDGE_LOOP ( 'NONE', ( #1186, #8320, #7688, #5000 ) ) ;
#3586 = EDGE_CURVE ( 'NONE', #5227, #7714, #495, .T. ) ;
#3587 = EDGE_CURVE ( 'NONE', #2971, #1524, #8537, .T. ) ;
#3588 = CARTESIAN_POINT ( 'NONE',  ( -50.00000000000004263, -425.0000000000000000, 3.469446951953614189E-15 ) ) ;
#3589 = CARTESIAN_POINT ( 'NONE',  ( 5.000000000000115463, -14.99999999999990230, -20.00000000000001776 ) ) ;
#3590 = EDGE_CURVE ( 'NONE', #3348, #3489, #589, .T. ) ;
#3591 = CARTESIAN_POINT ( 'NONE',  ( -1.310872448938785739, 8.480771745766666925, -0.3173508448888719413 ) ) ;
#3592 = ORIENTED_EDGE ( 'NONE', *, *, #2704, .F. ) ;
#3593 = CARTESIAN_POINT ( 'NONE',  ( 50.00000000000004263, 500.0000000000000000, -50.00000000000000000 ) ) ;
#3594 = CARTESIAN_POINT ( 'NONE',  ( -350.0000000000001137, 60.00000000000000000, -49.99999999999997158 ) ) ;
#3595 = ORIENTED_EDGE ( 'NONE', *, *, #3834, .F. ) ;
#3596 = CARTESIAN_POINT ( 'NONE',  ( -50.00000000000004263, 425.0000000000000000, 3.469446951953614189E-15 ) ) ;
#3597 = EDGE_LOOP ( 'NONE', ( #1281, #4112 ) ) ;
#3598 = CARTESIAN_POINT ( 'NONE',  ( 2.220446049250313081E-13, 9.237604307034075646, -8.400000000000018119 ) ) ;
#3599 = PLANE ( 'NONE',  #6502 ) ;
#3600 = EDGE_LOOP ( 'NONE', ( #6309, #6652, #1548 ) ) ;
#3601 = AXIS2_PLACEMENT_3D ( 'NONE', #6849, #8319, #2341 ) ;
#3602 = CARTESIAN_POINT ( 'NONE',  ( 5.000000000000004441, 2.342598717236861638, 4.057500000000047180 ) ) ;
#3603 = ORIENTED_EDGE ( 'NONE', *, *, #6676, .T. ) ;
#3604 = EDGE_LOOP ( 'NONE', ( #6045, #6521, #3691, #666 ) ) ;
#3605 = DIRECTION ( 'NONE',  ( 1.000000000000000000, 2.775557561562914622E-15, -3.821045009664285041E-30 ) ) ;
#3606 = LINE ( 'NONE', #6796, #7671 ) ;
#3607 = DIRECTION ( 'NONE',  ( 0.000000000000000000, 0.000000000000000000, -1.000000000000000000 ) ) ;
#3608 = EDGE_CURVE ( 'NONE', #6850, #8100, #3973, .T. ) ;
#3609 = CARTESIAN_POINT ( 'NONE',  ( -50.00000000000004263, 425.0000000000000000, -25.00000000000000355 ) ) ;
#3610 = CYLINDRICAL_SURFACE ( 'NONE', #6508, 4.499999999999983125 ) ;
#3611 = CARTESIAN_POINT ( 'NONE',  ( -6.661338147750939243E-13, 9.237604307034352757, 0.000000000000000000 ) ) ;
#3612 = ORIENTED_EDGE ( 'NONE', *, *, #8260, .F. ) ;
#3613 = AXIS2_PLACEMENT_3D ( 'NONE', #3138, #6417, #1649 ) ;
#3614 = CARTESIAN_POINT ( 'NONE',  ( 1.310872448937630219, -8.480771745766674030, -0.3173508448887735200 ) ) ;
#3615 = ORIENTED_EDGE ( 'NONE', *, *, #177, .T. ) ;
#3616 = VECTOR ( 'NONE', #7905, 1000.000000000000000 ) ;
#3617 = VECTOR ( 'NONE', #1119, 1000.000000000000000 ) ;
#3618 = CARTESIAN_POINT ( 'NONE',  ( 0.000000000000000000, 0.000000000000000000, 0.000000000000000000 ) ) ;
#3619 = EDGE_CURVE ( 'NONE', #8461, #1223, #6631, .T. ) ;
#3620 = VERTEX_POINT ( 'NONE', #2443 ) ;
#3621 = DIRECTION ( 'NONE',  ( 7.703719777548943412E-34, -0.000000000000000000, -1.000000000000000000 ) ) ;
#3622 = VERTEX_POINT ( 'NONE', #5094 ) ;
#3623 = VECTOR ( 'NONE', #978, 1000.000000000000114 ) ;
#3624 = AXIS2_PLACEMENT_3D ( 'NONE', #2127, #7433, #1464 ) ;
#3625 = ORIENTED_EDGE ( 'NONE', *, *, #1603, .T. ) ;
#3626 = AXIS2_PLACEMENT_3D ( 'NONE', #225, #4110, #6778 ) ;
#3627 = AXIS2_PLACEMENT_3D ( 'NONE', #6760, #6112, #3524 ) ;
#3628 = CIRCLE ( 'NONE', #8346, 9.499999999999998224 ) ;
#3629 = AXIS2_PLACEMENT_3D ( 'NONE', #1662, #4455, #5706 ) ;
#3630 = B_SPLINE_CURVE_WITH_KNOTS ( 'NONE', 3,
 ( #2337, #7618, #955, #2258, #1601, #3614, #6285, #294 ),
 .UNSPECIFIED., .F., .F.,
 ( 4, 2, 2, 4 ),
 ( 0.004673709593152060304, 0.005837709341827596564, 0.007001709090503132824, 0.009329708587854201873 ),
 .UNSPECIFIED. ) ;
#3631 = FILL_AREA_STYLE_COLOUR ( '', #1806 ) ;
#3632 = EDGE_CURVE ( 'NONE', #6135, #5665, #5470, .T. ) ;
#3633 = CIRCLE ( 'NONE', #4744, 15.00000000000002487 ) ;
#3634 = CARTESIAN_POINT ( 'NONE',  ( -8.000000000000664357, -1.555946510855793052, -8.332911297836323783 ) ) ;
#3635 = CARTESIAN_POINT ( 'NONE',  ( 5.080504117408890075, 2.106769544347818268, 0.000000000000000000 ) ) ;
#3636 = EDGE_LOOP ( 'NONE', ( #6804, #1213, #3562, #612, #1959, #3612 ) ) ;
#3637 = CARTESIAN_POINT ( 'NONE',  ( 8.000000000000007105, 4.618802153516954334, -8.400000000000018119 ) ) ;
#3638 = DIRECTION ( 'NONE',  ( 8.476012494971550862E-19, -1.514892278863297950E-17, 1.000000000000000000 ) ) ;
#3639 = ORIENTED_EDGE ( 'NONE', *, *, #5889, .F. ) ;
#3640 = DIRECTION ( 'NONE',  ( -7.703719777548943412E-34, 0.000000000000000000, 1.000000000000000000 ) ) ;
#3641 = ADVANCED_FACE ( 'NONE', ( #4488 ), #8496, .T. ) ;
#3642 = ORIENTED_EDGE ( 'NONE', *, *, #39, .T. ) ;
#3643 = DIRECTION ( 'NONE',  ( -1.540743955509788340E-33, 6.569728034446847052E-68, -1.000000000000000000 ) ) ;
#3644 = ADVANCED_FACE ( 'NONE', ( #4537 ), #5787, .F. ) ;
#3645 = CYLINDRICAL_SURFACE ( 'NONE', #8073, 4.499999999999997335 ) ;
#3646 = VERTEX_POINT ( 'NONE', #3835 ) ;
#3647 = DIRECTION ( 'NONE',  ( 0.000000000000000000, 0.000000000000000000, 1.000000000000000000 ) ) ;
#3648 = SHAPE_REPRESENTATION_RELATIONSHIP ( 'NONE' , 'NONE' ,  #2536, #3577 ) ;
#3649 = ORIENTED_EDGE ( 'NONE', *, *, #3308, .T. ) ;
#3650 = ORIENTED_EDGE ( 'NONE', *, *, #8047, .F. ) ;
#3651 = CARTESIAN_POINT ( 'NONE',  ( 0.000000000000000000, 0.000000000000000000, 5.559999999999998721 ) ) ;
#3652 = CARTESIAN_POINT ( 'NONE',  ( -44.99999999999992895, 500.0000000000000000, 50.00000000000000000 ) ) ;
#3653 = CIRCLE ( 'NONE', #2677, 50.00000000000008527 ) ;
#3654 = DIRECTION ( 'NONE',  ( 1.000000000000000000, 2.775557561562914622E-15, 0.000000000000000000 ) ) ;
#3655 = DIRECTION ( 'NONE',  ( 0.000000000000000000, 0.000000000000000000, -1.000000000000000000 ) ) ;
#3656 = DIRECTION ( 'NONE',  ( -1.000000000000000000, 1.774937036747276562E-30, 0.000000000000000000 ) ) ;
#3657 = DIRECTION ( 'NONE',  ( 0.000000000000000000, 0.000000000000000000, 1.000000000000000000 ) ) ;
#3658 = ORIENTED_EDGE ( 'NONE', *, *, #5491, .F. ) ;
#3659 = DIRECTION ( 'NONE',  ( -1.000000000000000000, 3.549874073494553124E-30, 0.000000000000000000 ) ) ;
#3660 = ORIENTED_EDGE ( 'NONE', *, *, #5716, .F. ) ;
#3661 = PRODUCT_RELATED_PRODUCT_CATEGORY ( 'part', '', ( #1050 ) ) ;
#3662 = VECTOR ( 'NONE', #1784, 999.9999999999998863 ) ;
#3663 = B_SPLINE_CURVE_WITH_KNOTS ( 'NONE', 3,
 ( #2992, #8269, #7569, #5488, #4301, #2210 ),
 .UNSPECIFIED., .F., .F.,
 ( 4, 2, 4 ),
 ( 0.008240550023493511955, 0.01057684187039398607, 0.01291313371729446192 ),
 .UNSPECIFIED. ) ;
#3664 = AXIS2_PLACEMENT_3D ( 'NONE', #6997, #3723, #8532 ) ;
#3665 = DIRECTION ( 'NONE',  ( -1.000000000000000000, 0.000000000000000000, 0.000000000000000000 ) ) ;
#3666 = FACE_OUTER_BOUND ( 'NONE', #7388, .T. ) ;
#3667 = ORIENTED_EDGE ( 'NONE', *, *, #2570, .T. ) ;
#3668 = AXIS2_PLACEMENT_3D ( 'NONE', #7752, #2528, #7885 ) ;
#3669 = ORIENTED_EDGE ( 'NONE', *, *, #8470, .F. ) ;
#3670 = ADVANCED_FACE ( 'NONE', ( #3270 ), #3797, .F. ) ;
#3671 = UNCERTAINTY_MEASURE_WITH_UNIT (LENGTH_MEASURE( 1.000000000000000082E-05 ), #513, 'distance_accuracy_value', 'NONE');
#3672 = DIRECTION ( 'NONE',  ( -0.8660254037844362651, -0.5000000000000039968, 0.000000000000000000 ) ) ;
#3673 = CARTESIAN_POINT ( 'NONE',  ( 0.000000000000000000, 0.000000000000000000, -8.400000000000018119 ) ) ;
#3674 = EDGE_LOOP ( 'NONE', ( #4253, #4809, #3552, #5634 ) ) ;
#3675 = CONICAL_SURFACE ( 'NONE', #609, 5.700000000000001954, 0.7853981633974472798 ) ;
#3676 = CARTESIAN_POINT ( 'NONE',  ( 0.000000000000000000, 415.0000000000000000, -5.551115123125782702E-14 ) ) ;
#3677 = CARTESIAN_POINT ( 'NONE',  ( 7.999999999999674039, -4.618802153517231446, -0.7145311798163467287 ) ) ;
#3678 = DIRECTION ( 'NONE',  ( 1.000000000000000000, -5.898059818321126865E-17, -4.579669976578766785E-16 ) ) ;
#3679 = ORIENTED_EDGE ( 'NONE', *, *, #3176, .F. ) ;
#3680 = CYLINDRICAL_SURFACE ( 'NONE', #6273, 5.500000000000023981 ) ;
#3681 = EDGE_CURVE ( 'NONE', #4082, #5338, #7875, .T. ) ;
#3682 = ORIENTED_EDGE ( 'NONE', *, *, #8558, .T. ) ;
#3683 = LINE ( 'NONE', #370, #1289 ) ;
#3684 = LINE ( 'NONE', #2411, #6538 ) ;
#3685 = ORIENTED_EDGE ( 'NONE', *, *, #5408, .F. ) ;
#3686 = CARTESIAN_POINT ( 'NONE',  ( 8.000000000000119016, 3.115336682266878654, -8.080606868608478877 ) ) ;
#3687 = LINE ( 'NONE', #5271, #8092 ) ;
#3688 =( LENGTH_UNIT ( ) NAMED_UNIT ( * ) SI_UNIT ( .MILLI., .METRE. ) );
#3689 = VERTEX_POINT ( 'NONE', #7890 ) ;
#3690 = EDGE_CURVE ( 'NONE', #3935, #2608, #1177, .T. ) ;
#3691 = ORIENTED_EDGE ( 'NONE', *, *, #341, .T. ) ;
#3692 = PRODUCT_DEFINITION_SHAPE ( 'NONE', 'NONE',  #4551 ) ;
#3693 = VERTEX_POINT ( 'NONE', #1880 ) ;
#3694 = CARTESIAN_POINT ( 'NONE',  ( -8.000000000000007105, -4.618802153517398423, -0.7145311798163467287 ) ) ;
#3695 = UNCERTAINTY_MEASURE_WITH_UNIT (LENGTH_MEASURE( 1.000000000000000082E-05 ), #528, 'distance_accuracy_value', 'NONE');
#3696 = CYLINDRICAL_SURFACE ( 'NONE', #5816, 5.500000000000024869 ) ;
#3697 =( NAMED_UNIT ( * ) SI_UNIT ( $, .STERADIAN. ) SOLID_ANGLE_UNIT ( ) );
#3698 = PLANE ( 'NONE',  #5029 ) ;
#3699 = EDGE_CURVE ( 'NONE', #4094, #2093, #8382, .T. ) ;
#3700 = CARTESIAN_POINT ( 'NONE',  ( -4.440892098500626162E-13, -9.237604307034018802, -0.7145311798163467287 ) ) ;
#3701 = APPLICATION_CONTEXT ( 'automotive_design' ) ;
#3702 = DIRECTION ( 'NONE',  ( 1.000000000000000000, -3.549874073494553124E-30, 0.000000000000000000 ) ) ;
#3703 = ORIENTED_EDGE ( 'NONE', *, *, #972, .F. ) ;
#3704 = CARTESIAN_POINT ( 'NONE',  ( 4.000000000000225597, -6.928203230275542523, 0.000000000000000000 ) ) ;
#3705 = ORIENTED_EDGE ( 'NONE', *, *, #5133, .F. ) ;
#3706 = VECTOR ( 'NONE', #109, 1000.000000000000000 ) ;
#3707 = DIRECTION ( 'NONE',  ( 1.000000000000000000, 0.000000000000000000, 0.000000000000000000 ) ) ;
#3708 = ITEM_DEFINED_TRANSFORMATION ( 'NONE', 'NONE', #6746,  #7563 ) ;
#3709 = EDGE_CURVE ( 'NONE', #5809, #3749, #2415, .T. ) ;
#3710 = FACE_OUTER_BOUND ( 'NONE', #5944, .T. ) ;
#3711 = ORIENTED_EDGE ( 'NONE', *, *, #2517, .F. ) ;
#3712 = CARTESIAN_POINT ( 'NONE',  ( 2.220446049250313081E-13, -0.8578643762688908936, 79.99999999999995737 ) ) ;
#3713 = AXIS2_PLACEMENT_3D ( 'NONE', #53, #7557, #5430 ) ;
#3714 = CARTESIAN_POINT ( 'NONE',  ( -8.000000000000007105, -4.618802153517065356, -8.400000000000018119 ) ) ;
#3715 = CARTESIAN_POINT ( 'NONE',  ( -2.644994884460003526, 7.710515798486560435, -0.08224679563998771314 ) ) ;
#3716 = DIRECTION ( 'NONE',  ( 3.851859888774471706E-33, -7.598173571352216173E-18, 1.000000000000000000 ) ) ;
#3717 = EDGE_CURVE ( 'NONE', #1999, #5555, #8419, .T. ) ;
#3718 = ORIENTED_EDGE ( 'NONE', *, *, #2987, .F. ) ;
#3719 = DIRECTION ( 'NONE',  ( -0.8660254037844365982, 0.5000000000000035527, -0.000000000000000000 ) ) ;
#3720 = CARTESIAN_POINT ( 'NONE',  ( 275.0000000000000000, -425.0000000000000000, -75.00000000000000000 ) ) ;
#3721 = APPLICATION_PROTOCOL_DEFINITION ( 'draft international standard', 'automotive_design', 1998, #5483 ) ;
#3722 = CIRCLE ( 'NONE', #1208, 5.500000000000024869 ) ;
#3723 = DIRECTION ( 'NONE',  ( 0.000000000000000000, 0.000000000000000000, 1.000000000000000000 ) ) ;
#3724 = DIRECTION ( 'NONE',  ( 1.000000000000000000, 0.000000000000000000, 0.000000000000000000 ) ) ;
#3725 = EDGE_CURVE ( 'NONE', #2603, #4358, #7282, .T. ) ;
#3726 = EDGE_LOOP ( 'NONE', ( #5056, #6947 ) ) ;
#3727 = DIRECTION ( 'NONE',  ( -1.000000000000000000, -3.083952846180992055E-15, 0.000000000000000000 ) ) ;
#3728 = ORIENTED_EDGE ( 'NONE', *, *, #8498, .F. ) ;
#3729 = CARTESIAN_POINT ( 'NONE',  ( 8.000000000000007105, 4.618802153516732290, -7.685468820183672278 ) ) ;
#3730 = ORIENTED_EDGE ( 'NONE', *, *, #795, .F. ) ;
#3731 = DIRECTION ( 'NONE',  ( 0.7071067811865474617, 2.508471778024696965E-30, -0.7071067811865474617 ) ) ;
#3732 = CARTESIAN_POINT ( 'NONE',  ( 275.0000000000000000, -425.0000000000000000, 0.000000000000000000 ) ) ;
#3733 = DIRECTION ( 'NONE',  ( 0.000000000000000000, 0.000000000000000000, 1.000000000000000000 ) ) ;
#3734 = EDGE_CURVE ( 'NONE', #4558, #569, #1561, .T. ) ;
#3735 = CIRCLE ( 'NONE', #8590, 8.000000000000007105 ) ;
#3736 = CARTESIAN_POINT ( 'NONE',  ( -44.99999999999992895, -425.0000000000000000, 3.122502256758253953E-15 ) ) ;
#3737 = CARTESIAN_POINT ( 'NONE',  ( 5.000000000000060396, -2.342598717236958006, -4.057500000000047180 ) ) ;
#3738 = CARTESIAN_POINT ( 'NONE',  ( -2.645508037662050338, -7.710219529346595380, -0.06809871960545571534 ) ) ;
#3739 = LINE ( 'NONE', #6973, #6896 ) ;
#3740 = DIRECTION ( 'NONE',  ( -1.000000000000000000, 1.284024588418159550E-35, 0.000000000000000000 ) ) ;
#3741 = ORIENTED_EDGE ( 'NONE', *, *, #1148, .T. ) ;
#3742 = EDGE_CURVE ( 'NONE', #3286, #650, #1710, .T. ) ;
#3743 = DIRECTION ( 'NONE',  ( 6.400024471206993532E-36, -1.000000000000000000, -7.598173571352311699E-18 ) ) ;
#3744 = VERTEX_POINT ( 'NONE', #3313 ) ;
#3745 = ADVANCED_FACE ( 'NONE', ( #4675 ), #2714, .T. ) ;
#3746 = FACE_OUTER_BOUND ( 'NONE', #3464, .T. ) ;
#3747 = VECTOR ( 'NONE', #6661, 1000.000000000000000 ) ;
#3748 = CARTESIAN_POINT ( 'NONE',  ( 3.318518101602915493, 7.321656987762904301, -8.400000000000034106 ) ) ;
#3749 = VERTEX_POINT ( 'NONE', #34 ) ;
#3750 = CARTESIAN_POINT ( 'NONE',  ( 4.250000000000000888, -32.50000000000004974, -1.504632769052525000E-32 ) ) ;
#3751 = ADVANCED_FACE ( 'NONE', ( #2815 ), #2896, .F. ) ;
#3752 = VECTOR ( 'NONE', #8290, 1000.000000000000000 ) ;
#3753 = CIRCLE ( 'NONE', #5420, 4.250000000000007105 ) ;
#3754 = FACE_OUTER_BOUND ( 'NONE', #3181, .T. ) ;
#3755 = CIRCLE ( 'NONE', #1244, 25.00000000000000711 ) ;
#3756 = DIRECTION ( 'NONE',  ( 0.000000000000000000, -5.322451846059955323E-30, 1.000000000000000000 ) ) ;
#3757 = PLANE ( 'NONE',  #2908 ) ;
#3758 = ORIENTED_EDGE ( 'NONE', *, *, #5341, .T. ) ;
#3759 = AXIS2_PLACEMENT_3D ( 'NONE', #86, #4811, #800 ) ;
#3760 = CARTESIAN_POINT ( 'NONE',  ( 44.99999999999992895, -500.0000000000000000, 50.00000000000000000 ) ) ;
#3761 = CARTESIAN_POINT ( 'NONE',  ( 0.000000000000000000, 0.000000000000000000, -8.400000000000018119 ) ) ;
#3762 =( NAMED_UNIT ( * ) PLANE_ANGLE_UNIT ( ) SI_UNIT ( $, .RADIAN. ) );
#3763 = EDGE_CURVE ( 'NONE', #3886, #8340, #15, .T. ) ;
#3764 = CARTESIAN_POINT ( 'NONE',  ( 0.000000000000000000, -3.469446951953614189E-15, 130.0000000000000000 ) ) ;
#3765 = EDGE_CURVE ( 'NONE', #4846, #2214, #3110, .T. ) ;
#3766 = COLOUR_RGB ( '',0.7921568627450980005, 0.8196078431372548767, 0.9333333333333333481 ) ;
#3767 = CARTESIAN_POINT ( 'NONE',  ( 36.74999999999997868, 1.439826269745208429E-14, 18.00000000000000355 ) ) ;
#3768 = VERTEX_POINT ( 'NONE', #2135 ) ;
#3769 = CARTESIAN_POINT ( 'NONE',  ( 139.1719999999995423, 3.530679291910986181E-14, -5.000000000001512568 ) ) ;
#3770 = ORIENTED_EDGE ( 'NONE', *, *, #985, .F. ) ;
#3771 = CARTESIAN_POINT ( 'NONE',  ( 5.080504117408889186, 2.106769544347817824, -8.400000000000018119 ) ) ;
#3772 = ORIENTED_EDGE ( 'NONE', *, *, #3619, .T. ) ;
#3773 = DIRECTION ( 'NONE',  ( 0.8660254037844367092, -0.5000000000000033307, 0.000000000000000000 ) ) ;
#3774 = EDGE_CURVE ( 'NONE', #5857, #863, #7391, .T. ) ;
#3775 = AXIS2_PLACEMENT_3D ( 'NONE', #1695, #4409, #6300 ) ;
#3776 = DIRECTION ( 'NONE',  ( -0.9237280213470678847, -0.3830490080632384942, 0.000000000000000000 ) ) ;
#3777 = CARTESIAN_POINT ( 'NONE',  ( 0.000000000000000000, 0.000000000000000000, 0.000000000000000000 ) ) ;
#3778 = DIRECTION ( 'NONE',  ( -1.000000000000000000, 0.000000000000000000, 0.000000000000000000 ) ) ;
#3779 = CARTESIAN_POINT ( 'NONE',  ( -8.000000000000007105, -4.618802153517065356, -7.685468820183672278 ) ) ;
#3780 = CARTESIAN_POINT ( 'NONE',  ( 8.000000000000007105, 4.618802153517065356, -7.685468820183672278 ) ) ;
#3781 = CARTESIAN_POINT ( 'NONE',  ( 8.400000000000018119, -5.551115123125782702E-14, 6.661338147750939243E-13 ) ) ;
#3782 = ORIENTED_EDGE ( 'NONE', *, *, #1415, .F. ) ;
#3783 = FILL_AREA_STYLE ('',( #1815 ) ) ;
#3784 = EDGE_LOOP ( 'NONE', ( #8265, #1459, #1783, #8545 ) ) ;
#3785 = ADVANCED_FACE ( 'NONE', ( #4207 ), #2900, .F. ) ;
#3786 = CARTESIAN_POINT ( 'NONE',  ( 2.309976723937862797, -7.903938623647071005, -0.1306530452039634804 ) ) ;
#3787 = CARTESIAN_POINT ( 'NONE',  ( 0.000000000000000000, 415.0000000000000000, -5.551115123125782702E-14 ) ) ;
#3788 = DIRECTION ( 'NONE',  ( 1.000000000000000000, 0.000000000000000000, 0.000000000000000000 ) ) ;
#3789 = VERTEX_POINT ( 'NONE', #4785 ) ;
#3790 = EDGE_LOOP ( 'NONE', ( #8491, #519, #1549, #7462, #5645, #832, #4157, #627, #5413, #1162 ) ) ;
#3791 = CARTESIAN_POINT ( 'NONE',  ( -49.99999999999954525, 120.0000000000003268, 0.000000000000000000 ) ) ;
#3792 = EDGE_CURVE ( 'NONE', #5906, #5923, #610, .T. ) ;
#3793 = EDGE_CURVE ( 'NONE', #863, #5176, #3029, .T. ) ;
#3794 = AXIS2_PLACEMENT_3D ( 'NONE', #997, #2330, #8387 ) ;
#3795 = DIRECTION ( 'NONE',  ( 0.000000000000000000, -5.322451846059955323E-30, 1.000000000000000000 ) ) ;
#3796 = ORIENTED_EDGE ( 'NONE', *, *, #6904, .T. ) ;
#3797 = CYLINDRICAL_SURFACE ( 'NONE', #3518, 5.500000000000024869 ) ;
#3798 = DIRECTION ( 'NONE',  ( 1.000000000000000000, 8.881784197001244435E-16, 0.000000000000000000 ) ) ;
#3799 = DIRECTION ( 'NONE',  ( 3.919652622816902408E-30, 3.944304526105059027E-30, -1.000000000000000000 ) ) ;
#3800 = APPLICATION_PROTOCOL_DEFINITION ( 'draft international standard', 'automotive_design', 1998, #1909 ) ;
#3801 = CIRCLE ( 'NONE', #468, 10.50000000000002132 ) ;
#3802 = AXIS2_PLACEMENT_3D ( 'NONE', #5253, #2640, #4123 ) ;
#3803 = DIRECTION ( 'NONE',  ( 1.000000000000000000, -1.284024588418159817E-35, 0.000000000000000000 ) ) ;
#3804 = ORIENTED_EDGE ( 'NONE', *, *, #394, .F. ) ;
#3805 = CARTESIAN_POINT ( 'NONE',  ( 8.000000000000122569, 0.7809653281574663319, -8.399999999999955946 ) ) ;
#3806 = EDGE_LOOP ( 'NONE', ( #4930, #1933, #7641, #8233 ) ) ;
#3807 = AXIS2_PLACEMENT_3D ( 'NONE', #6577, #1441, #3352 ) ;
#3808 = AXIS2_PLACEMENT_3D ( 'NONE', #6594, #1273, #8034 ) ;
#3809 = CARTESIAN_POINT ( 'NONE',  ( 4.000000000000003553, 9.714451465470119729E-14, 0.000000000000000000 ) ) ;
#3810 = ORIENTED_EDGE ( 'NONE', *, *, #4663, .T. ) ;
#3811 = FACE_OUTER_BOUND ( 'NONE', #2502, .T. ) ;
#3812 = CARTESIAN_POINT ( 'NONE',  ( 0.000000000000000000, 299.9999999999999432, -6.938893903907228378E-14 ) ) ;
#3813 = CARTESIAN_POINT ( 'NONE',  ( 0.000000000000000000, 410.0000000000000000, -5.551115123125782702E-14 ) ) ;
#3814 = CARTESIAN_POINT ( 'NONE',  ( -44.99999999999992895, -425.0000000000000000, 3.122502256758253953E-15 ) ) ;
#3815 = DIRECTION ( 'NONE',  ( 0.5000000000000035527, 0.8660254037844365982, 0.000000000000000000 ) ) ;
#3816 = AXIS2_PLACEMENT_3D ( 'NONE', #827, #3347, #4490 ) ;
#3817 = CARTESIAN_POINT ( 'NONE',  ( -54.49999999999968736, 87.50000000000034106, -1.942890293094024198E-13 ) ) ;
#3818 = ADVANCED_FACE ( 'NONE', ( #4340 ), #5325, .T. ) ;
#3819 = CARTESIAN_POINT ( 'NONE',  ( 3.999999999999337419, -6.928203230275431501, 0.000000000000000000 ) ) ;
#3820 = ORIENTED_EDGE ( 'NONE', *, *, #8339, .F. ) ;
#3821 = ORIENTED_EDGE ( 'NONE', *, *, #916, .T. ) ;
#3822 = CIRCLE ( 'NONE', #1457, 69.99999999999998579 ) ;
#3823 = DIRECTION ( 'NONE',  ( -0.000000000000000000, -0.000000000000000000, 1.000000000000000000 ) ) ;
#3824 = EDGE_CURVE ( 'NONE', #4276, #896, #2841, .T. ) ;
#3825 = CARTESIAN_POINT ( 'NONE',  ( -19.99999999999982947, 15.00000000000012434, 10.00000000000000888 ) ) ;
#3826 = ADVANCED_FACE ( 'NONE', ( #3811 ), #2457, .T. ) ;
#3827 = VERTEX_POINT ( 'NONE', #3651 ) ;
#3828 = CARTESIAN_POINT ( 'NONE',  ( 4.000000000000003553, -1.759474945355339992, -3.047499999999869758 ) ) ;
#3829 = EDGE_LOOP ( 'NONE', ( #6157, #5735 ) ) ;
#3830 = FACE_OUTER_BOUND ( 'NONE', #2848, .T. ) ;
#3831 = DIRECTION ( 'NONE',  ( 0.000000000000000000, -5.322451846059955323E-30, 1.000000000000000000 ) ) ;
#3832 = DIRECTION ( 'NONE',  ( 0.000000000000000000, 0.000000000000000000, -1.000000000000000000 ) ) ;
#3833 = VERTEX_POINT ( 'NONE', #7766 ) ;
#3834 = EDGE_CURVE ( 'NONE', #8292, #1989, #5465, .T. ) ;
#3835 = CARTESIAN_POINT ( 'NONE',  ( 36.74999999999997868, 1.439826269745208429E-14, -1.203706215242020903E-32 ) ) ;
#3836 = DIRECTION ( 'NONE',  ( -3.851859888774471706E-33, 7.598173571352219255E-18, -1.000000000000000000 ) ) ;
#3837 = DIRECTION ( 'NONE',  ( 1.000000000000000000, 0.000000000000000000, 0.000000000000000000 ) ) ;
#3838 = COLOUR_RGB ( '',0.7921568627450980005, 0.8196078431372548767, 0.9333333333333333481 ) ;
#3839 = LINE ( 'NONE', #2430, #2553 ) ;
#3840 = EDGE_CURVE ( 'NONE', #7453, #7966, #1151, .T. ) ;
#3841 = ORIENTED_EDGE ( 'NONE', *, *, #8248, .F. ) ;
#3842 = AXIS2_PLACEMENT_3D ( 'NONE', #5804, #5110, #4389 ) ;
#3843 = CARTESIAN_POINT ( 'NONE',  ( -31.74999999999994316, 6.123233995735102772E-16, -5.000000000000034639 ) ) ;
#3844 = VERTEX_POINT ( 'NONE', #8465 ) ;
#3845 = FACE_OUTER_BOUND ( 'NONE', #6903, .T. ) ;
#3846 = ORIENTED_EDGE ( 'NONE', *, *, #2912, .T. ) ;
#3847 = CARTESIAN_POINT ( 'NONE',  ( -275.0000000000000000, 425.0000000000000000, 80.00000000000015632 ) ) ;
#3848 = PRODUCT_DEFINITION_CONTEXT ( 'detailed design', #1909, 'design' ) ;
#3849 = CARTESIAN_POINT ( 'NONE',  ( 0.000000000000000000, 1.759474945355512965, -3.047500000000091802 ) ) ;
#3850 = CARTESIAN_POINT ( 'NONE',  ( 4.000000000000003553, -1.759474945355333109, 3.047500000000091802 ) ) ;
#3851 = DIRECTION ( 'NONE',  ( -1.000000000000000000, 0.000000000000000000, 0.000000000000000000 ) ) ;
#3852 = FACE_OUTER_BOUND ( 'NONE', #1679, .T. ) ;
#3853 = CARTESIAN_POINT ( 'NONE',  ( 5.000000000000004441, 4.685197434473897360, 0.000000000000000000 ) ) ;
#3854 = CARTESIAN_POINT ( 'NONE',  ( 5.000000000000004441, 0.000000000000000000, 0.000000000000000000 ) ) ;
#3855 = ORIENTED_EDGE ( 'NONE', *, *, #7344, .F. ) ;
#3856 = CARTESIAN_POINT ( 'NONE',  ( -49.99999999999953815, 120.0000000000003268, 9.999999999999980460 ) ) ;
#3857 = ORIENTED_EDGE ( 'NONE', *, *, #1330, .F. ) ;
#3858 = DIRECTION ( 'NONE',  ( 0.000000000000000000, 0.000000000000000000, -1.000000000000000000 ) ) ;
#3859 = EDGE_CURVE ( 'NONE', #5854, #5405, #5610, .T. ) ;
#3860 = PLANE ( 'NONE',  #7602 ) ;
#3861 = DIRECTION ( 'NONE',  ( 0.000000000000000000, 0.000000000000000000, -1.000000000000000000 ) ) ;
#3862 = ORIENTED_EDGE ( 'NONE', *, *, #2178, .T. ) ;
#3863 = CARTESIAN_POINT ( 'NONE',  ( 275.0000000000000000, 425.0000000000000000, -79.99999999999984368 ) ) ;
#3864 = EDGE_LOOP ( 'NONE', ( #3649, #1495, #2874, #6155 ) ) ;
#3865 = DIRECTION ( 'NONE',  ( 0.9237280213470678847, 0.3830490080632384942, 0.000000000000000000 ) ) ;
#3866 = ORIENTED_EDGE ( 'NONE', *, *, #5774, .F. ) ;
#3867 = FACE_OUTER_BOUND ( 'NONE', #6354, .T. ) ;
#3868 = EDGE_LOOP ( 'NONE', ( #4860, #5039, #4398, #5934, #4262 ) ) ;
#3869 = EDGE_CURVE ( 'NONE', #1068, #18, #7043, .T. ) ;
#3870 = CARTESIAN_POINT ( 'NONE',  ( -5.500000000000000000, 6.735557395310442023E-16, -45.00000000000000711 ) ) ;
#3871 = VECTOR ( 'NONE', #5283, 1000.000000000000000 ) ;
#3872 = CIRCLE ( 'NONE', #5562, 24.49999999999999645 ) ;
#3873 = CARTESIAN_POINT ( 'NONE',  ( -12.99999999999956124, 120.0000000000003411, 9.999999999999980460 ) ) ;
#3874 = DIRECTION ( 'NONE',  ( 3.919652622816902408E-30, 3.944304526105059027E-30, -1.000000000000000000 ) ) ;
#3875 = VERTEX_POINT ( 'NONE', #7123 ) ;
#3876 = CARTESIAN_POINT ( 'NONE',  ( -1.313474075707541822, -8.479269695851096245, -8.083279549040014444 ) ) ;
#3877 = PRODUCT_CONTEXT ( 'NONE', #4138, 'mechanical' ) ;
#3878 = AXIS2_PLACEMENT_3D ( 'NONE', #2453, #3023, #5102 ) ;
#3879 = EDGE_CURVE ( 'NONE', #7819, #4220, #1687, .T. ) ;
#3880 = CONICAL_SURFACE ( 'NONE', #3056, 8.000000000000007105, 1.047197551196597631 ) ;
#3881 = FACE_OUTER_BOUND ( 'NONE', #7203, .T. ) ;
#3882 = ORIENTED_EDGE ( 'NONE', *, *, #4088, .F. ) ;
#3883=STYLED_ITEM('',(#8677),#20);
#3884 = LINE ( 'NONE', #5379, #989 ) ;
#3885 = AXIS2_PLACEMENT_3D ( 'NONE', #6176, #2932, #7679 ) ;
#3886 = VERTEX_POINT ( 'NONE', #7005 ) ;
#3887 = EDGE_CURVE ( 'NONE', #5176, #698, #1039, .T. ) ;
#3888 = LINE ( 'NONE', #8385, #5627 ) ;
#3889 = PRODUCT_DEFINITION_SHAPE ( 'NONE', 'NONE',  #4926 ) ;
#3890 = ORIENTED_EDGE ( 'NONE', *, *, #5716, .T. ) ;
#3891 = CARTESIAN_POINT ( 'NONE',  ( 5.355005115540952154, 6.145890662064715571, -8.317753204360256447 ) ) ;
#3892 = CIRCLE ( 'NONE', #3629, 8.000000000000007105 ) ;
#3893=STYLED_ITEM('',(#8670),#5834);
#3894 = CARTESIAN_POINT ( 'NONE',  ( 9.999999999999896971, 0.000000000000000000, 0.000000000000000000 ) ) ;
#3895 = DIRECTION ( 'NONE',  ( -1.000000000000000000, -8.881784197001244435E-16, 0.000000000000000000 ) ) ;
#3896 = DIRECTION ( 'NONE',  ( 1.000000000000000000, 8.881784197001244435E-16, 0.000000000000000000 ) ) ;
#3897=STYLED_ITEM('',(#8656),#2963);
#3898 = DIRECTION ( 'NONE',  ( 1.000000000000000000, 3.083952846180997183E-15, 0.000000000000000000 ) ) ;
#3899 = DIRECTION ( 'NONE',  ( -5.423418723394458790E-31, 0.8660254037844379305, -0.5000000000000014433 ) ) ;
#3900 = FACE_OUTER_BOUND ( 'NONE', #6229, .T. ) ;
#3901 = ORIENTED_EDGE ( 'NONE', *, *, #916, .F. ) ;
#3902 = ORIENTED_EDGE ( 'NONE', *, *, #8462, .F. ) ;
#3903 = DIRECTION ( 'NONE',  ( -3.919652622816902408E-30, -3.944304526105059027E-30, 1.000000000000000000 ) ) ;
#3904 = PRESENTATION_STYLE_ASSIGNMENT (( #3341 ) ) ;
#3905 = CARTESIAN_POINT ( 'NONE',  ( -5.354491962338047806, 6.146186931204369763, -0.06809871960538080304 ) ) ;
#3906 = ORIENTED_EDGE ( 'NONE', *, *, #5444, .T. ) ;
#3907 = DIRECTION ( 'NONE',  ( -1.000000000000000000, -8.881784197001244435E-16, 0.000000000000000000 ) ) ;
#3908 = EDGE_LOOP ( 'NONE', ( #4614, #6053 ) ) ;
#3909 = ADVANCED_FACE ( 'NONE', ( #5027 ), #7985, .T. ) ;
#3910 = VERTEX_POINT ( 'NONE', #7728 ) ;
#3911 = FACE_BOUND ( 'NONE', #2096, .T. ) ;
#3912 = EDGE_LOOP ( 'NONE', ( #7424, #4772, #1668, #6975 ) ) ;
#3913 = CARTESIAN_POINT ( 'NONE',  ( -4.000000000000003553, -6.928203230275431501, -8.400000000000018119 ) ) ;
#3914 = PLANE ( 'NONE',  #6054 ) ;
#3915 = AXIS2_PLACEMENT_3D ( 'NONE', #2481, #5631, #6232 ) ;
#3916 = CARTESIAN_POINT ( 'NONE',  ( 5.000000000000004441, 0.000000000000000000, 0.000000000000000000 ) ) ;
#3917 = ORIENTED_EDGE ( 'NONE', *, *, #4884, .T. ) ;
#3918 = VECTOR ( 'NONE', #5905, 1000.000000000000000 ) ;
#3919 = DIRECTION ( 'NONE',  ( -1.000000000000000000, -8.881784197001244435E-16, 0.000000000000000000 ) ) ;
#3920 = ADVANCED_FACE ( 'NONE', ( #1758 ), #2371, .F. ) ;
#3921 = APPLICATION_PROTOCOL_DEFINITION ( 'draft international standard', 'automotive_design', 1998, #3701 ) ;
#3922 = AXIS2_PLACEMENT_3D ( 'NONE', #194, #4824, #1506 ) ;
#3923 = VECTOR ( 'NONE', #7843, 1000.000000000000000 ) ;
#3924 = LINE ( 'NONE', #7287, #2409 ) ;
#3925 = CONICAL_SURFACE ( 'NONE', #3095, 3.309499999999999886, 0.7853981633975651855 ) ;
#3926 = DIRECTION ( 'NONE',  ( -0.000000000000000000, -1.000000000000000000, -1.795949010423047374E-16 ) ) ;
#3927 = ORIENTED_EDGE ( 'NONE', *, *, #6427, .F. ) ;
#3928 = CYLINDRICAL_SURFACE ( 'NONE', #5296, 8.000000000000000000 ) ;
#3929 = EDGE_CURVE ( 'NONE', #4220, #4181, #3072, .T. ) ;
#3930 = CIRCLE ( 'NONE', #6183, 75.00000000000000000 ) ;
#3931 = CIRCLE ( 'NONE', #7560, 75.00000000000005684 ) ;
#3932 = FACE_OUTER_BOUND ( 'NONE', #6566, .T. ) ;
#3933 = VERTEX_POINT ( 'NONE', #2418 ) ;
#3934 = CARTESIAN_POINT ( 'NONE',  ( 0.000000000000000000, 9.237604307034130713, -7.685468820183672278 ) ) ;
#3935 = VERTEX_POINT ( 'NONE', #676 ) ;
#3936 = TOROIDAL_SURFACE ( 'NONE', #3390, 5.400000000000034994, 0.4000000000000000222 ) ;
#3937 = CARTESIAN_POINT ( 'NONE',  ( 4.680456609904013909, 6.535341423375667702, -8.383111142572204244 ) ) ;
#3938 = AXIS2_PLACEMENT_3D ( 'NONE', #8185, #1604, #5592 ) ;
#3939 = CARTESIAN_POINT ( 'NONE',  ( 50.00000000000004263, 500.0000000000000000, 45.00000000000000711 ) ) ;
#3940 = CARTESIAN_POINT ( 'NONE',  ( 4.000000000000003553, 9.751772576674139373E-14, -3.047499999999999876 ) ) ;
#3941 = DIRECTION ( 'NONE',  ( 0.000000000000000000, 0.000000000000000000, -1.000000000000000000 ) ) ;
#3942 = VECTOR ( 'NONE', #621, 1000.000000000000000 ) ;
#3943 = FACE_BOUND ( 'NONE', #419, .T. ) ;
#3944 = AXIS2_PLACEMENT_3D ( 'NONE', #7616, #1635, #6974 ) ;
#3945 = ADVANCED_FACE ( 'NONE', ( #5203 ), #4505, .T. ) ;
#3946 = CARTESIAN_POINT ( 'NONE',  ( 7.347286611337029427, 4.995646404165263732, -0.4969600502617758098 ) ) ;
#3947 = VERTEX_POINT ( 'NONE', #2633 ) ;
#3948 = FACE_BOUND ( 'NONE', #7617, .T. ) ;
#3949 = ORIENTED_EDGE ( 'NONE', *, *, #866, .T. ) ;
#3950 = DIRECTION ( 'NONE',  ( 0.5000000000000035527, 0.8660254037844365982, 0.000000000000000000 ) ) ;
#3951 = FACE_BOUND ( 'NONE', #8129, .T. ) ;
#3952 = UNCERTAINTY_MEASURE_WITH_UNIT (LENGTH_MEASURE( 1.000000000000000082E-05 ), #3224, 'distance_accuracy_value', 'NONE');
#3953 = AXIS2_PLACEMENT_3D ( 'NONE', #3462, #6902, #6946 ) ;
#3954 = DIRECTION ( 'NONE',  ( -6.938893903907228378E-17, 0.000000000000000000, 1.000000000000000000 ) ) ;
#3955 = DIRECTION ( 'NONE',  ( -3.851859888774471706E-33, -1.232595164407830946E-32, -1.000000000000000000 ) ) ;
#3956 = EDGE_CURVE ( 'NONE', #1071, #6230, #2023, .T. ) ;
#3957 = CARTESIAN_POINT ( 'NONE',  ( 0.000000000000000000, 0.000000000000000000, -8.400000000000018119 ) ) ;
#3958 = CARTESIAN_POINT ( 'NONE',  ( -4.681481898396918417, 6.534749472788111468, 4.815212898551246568E-14 ) ) ;
#3959 = CARTESIAN_POINT ( 'NONE',  ( 2.644994884459374695, -7.710515798486562211, -8.317753204360146313 ) ) ;
#3960 = CARTESIAN_POINT ( 'NONE',  ( -8.000000000000229150, 4.618802153516954334, -7.685468820183672278 ) ) ;
#3961 = ORIENTED_EDGE ( 'NONE', *, *, #7230, .T. ) ;
#3962 = PRODUCT_DEFINITION_FORMATION_WITH_SPECIFIED_SOURCE ( 'ANY', '', #5872, .NOT_KNOWN. ) ;
#3963 = ORIENTED_EDGE ( 'NONE', *, *, #5774, .T. ) ;
#3964 = DIRECTION ( 'NONE',  ( -1.774937036747276562E-30, 1.000000000000000000, -1.110768649713241713E-15 ) ) ;
#3965 = VERTEX_POINT ( 'NONE', #3847 ) ;
#3966 = LINE ( 'NONE', #3400, #602 ) ;
#3967 = VECTOR ( 'NONE', #4467, 1000.000000000000000 ) ;
#3968 = CARTESIAN_POINT ( 'NONE',  ( -54.49999999999963762, 87.50000000000034106, 9.999999999999786837 ) ) ;
#3969 = EDGE_CURVE ( 'NONE', #6584, #2762, #2590, .T. ) ;
#3970 = CARTESIAN_POINT ( 'NONE',  ( 5.000000000000004441, -2.342598717236951789, 4.057500000000047180 ) ) ;
#3971 = DIRECTION ( 'NONE',  ( 1.000000000000000000, -0.000000000000000000, -6.938893903907228378E-17 ) ) ;
#3972 = ORIENTED_EDGE ( 'NONE', *, *, #710, .T. ) ;
#3973 = LINE ( 'NONE', #4447, #3662 ) ;
#3974 =( REPRESENTATION_RELATIONSHIP ('NONE','NONE', #1279, #7270 ) REPRESENTATION_RELATIONSHIP_WITH_TRANSFORMATION ( #1205 )SHAPE_REPRESENTATION_RELATIONSHIP( ) );
#3975 = PRODUCT_CONTEXT ( 'NONE', #5661, 'mechanical' ) ;
#3976 = CARTESIAN_POINT ( 'NONE',  ( 10.40000000000001990, 6.613092715395462920E-16, 5.400000000000479083 ) ) ;
#3977 = ADVANCED_FACE ( 'NONE', ( #5963 ), #3238, .T. ) ;
#3978 = ORIENTED_EDGE ( 'NONE', *, *, #5829, .T. ) ;
#3979 = DIRECTION ( 'NONE',  ( 3.919652622816902408E-30, 3.944304526105059027E-30, -1.000000000000000000 ) ) ;
#3980 = ORIENTED_EDGE ( 'NONE', *, *, #3573, .T. ) ;
#3981 = CARTESIAN_POINT ( 'NONE',  ( 4.000000000000003553, 6.928203230275431501, -8.400000000000018119 ) ) ;
#3982 = ORIENTED_EDGE ( 'NONE', *, *, #3793, .F. ) ;
#3983 = CARTESIAN_POINT ( 'NONE',  ( 6.686525924292488376, -5.377136764700389371, -8.083279549040231160 ) ) ;
#3984 = EDGE_CURVE ( 'NONE', #4330, #6381, #4446, .T. ) ;
#3985 = DIRECTION ( 'NONE',  ( -1.000000000000000000, -8.881784197001244435E-16, 0.000000000000000000 ) ) ;
#3986 = CARTESIAN_POINT ( 'NONE',  ( -8.000000000000007105, 0.000000000000000000, 0.000000000000000000 ) ) ;
#3987 = CARTESIAN_POINT ( 'NONE',  ( 0.000000000000000000, 9.237604307034130713, -8.400000000000018119 ) ) ;
#3988 = DIRECTION ( 'NONE',  ( 1.000000000000000000, -1.284024588418159550E-35, 0.000000000000000000 ) ) ;
#3989 = ORIENTED_EDGE ( 'NONE', *, *, #2119, .T. ) ;
#3990 = DIRECTION ( 'NONE',  ( 1.000000000000000000, 2.775557561562898056E-15, -3.821045009664285041E-30 ) ) ;
#3991 = ORIENTED_EDGE ( 'NONE', *, *, #8104, .F. ) ;
#3992 = FACE_OUTER_BOUND ( 'NONE', #3600, .T. ) ;
#3993 = AXIS2_PLACEMENT_3D ( 'NONE', #4299, #1442, #4097 ) ;
#3994 = EDGE_CURVE ( 'NONE', #6524, #1524, #6689, .T. ) ;
#3995 = CARTESIAN_POINT ( 'NONE',  ( 5.354491962337974975, -6.146186931204550064, -0.06809871960543639746 ) ) ;
#3996 = DIRECTION ( 'NONE',  ( 1.463706757734299248E-32, -1.000000000000000000, 4.930380657631321594E-32 ) ) ;
#3997 = DIRECTION ( 'NONE',  ( 1.000000000000000000, 2.775557561562892140E-15, 0.000000000000000000 ) ) ;
#3998 = CARTESIAN_POINT ( 'NONE',  ( 0.000000000000000000, -299.9999999999999432, -2.775557561562891351E-14 ) ) ;
#3999 = ORIENTED_EDGE ( 'NONE', *, *, #8040, .T. ) ;
#4000 = DIRECTION ( 'NONE',  ( 0.000000000000000000, 0.000000000000000000, 1.000000000000000000 ) ) ;
#4001 = ORIENTED_EDGE ( 'NONE', *, *, #98, .F. ) ;
#4002 = CARTESIAN_POINT ( 'NONE',  ( -7.999999999999892530, -0.7805016046292091447, -8.400000000000073186 ) ) ;
#4003 = SHAPE_REPRESENTATION ( 'flat washer narrow_am_B18.22M - Plain washer, 10 mm, narrow', ( #7563 ), #4924 ) ;
#4004 = CARTESIAN_POINT ( 'NONE',  ( 0.000000000000000000, 0.000000000000000000, 0.000000000000000000 ) ) ;
#4005 = CARTESIAN_POINT ( 'NONE',  ( -2.644994884459267226, 7.710515798486376582, -0.08224679563975054175 ) ) ;
#4006 = FACE_BOUND ( 'NONE', #2307, .T. ) ;
#4007 = DIRECTION ( 'NONE',  ( 6.400024471206997542E-36, -1.000000000000000000, -7.598173571352217714E-18 ) ) ;
#4008 = DIRECTION ( 'NONE',  ( 1.000000000000000000, 0.000000000000000000, 0.000000000000000000 ) ) ;
#4009 = ORIENTED_EDGE ( 'NONE', *, *, #6314, .F. ) ;
#4010 = DIRECTION ( 'NONE',  ( -0.5000000000000041078, 0.8660254037844363761, 0.000000000000000000 ) ) ;
#4011 = ORIENTED_EDGE ( 'NONE', *, *, #3590, .F. ) ;
#4012 = SHAPE_DEFINITION_REPRESENTATION ( #4519, #4003 ) ;
#4013 = EDGE_CURVE ( 'NONE', #6876, #1496, #5293, .T. ) ;
#4014 = CONICAL_SURFACE ( 'NONE', #3040, 8.000000000000007105, 1.047197551196597631 ) ;
#4015 = DIRECTION ( 'NONE',  ( -7.703719777548943412E-34, 0.000000000000000000, 1.000000000000000000 ) ) ;
#4016 = EDGE_LOOP ( 'NONE', ( #5883, #3972, #741, #4943 ) ) ;
#4017 = VECTOR ( 'NONE', #7309, 1000.000000000000000 ) ;
#4018 = DIRECTION ( 'NONE',  ( 3.919652622816902408E-30, 3.944304526105059027E-30, -1.000000000000000000 ) ) ;
#4019 = AXIS2_PLACEMENT_3D ( 'NONE', #1598, #4260, #8353 ) ;
#4020 = VECTOR ( 'NONE', #8168, 1000.000000000000000 ) ;
#4021 = VERTEX_POINT ( 'NONE', #7334 ) ;
#4022 = EDGE_CURVE ( 'NONE', #7189, #7833, #5053, .T. ) ;
#4023 = EDGE_CURVE ( 'NONE', #6303, #6735, #6055, .T. ) ;
#4024 = CARTESIAN_POINT ( 'NONE',  ( 4.680456609903968612, 6.535341423375565562, -8.383111142572266417 ) ) ;
#4025 = ORIENTED_EDGE ( 'NONE', *, *, #4549, .F. ) ;
#4026 = CARTESIAN_POINT ( 'NONE',  ( -6.689127551062048482, -5.375634714784658819, -0.3173508448886869227 ) ) ;
#4027 = AXIS2_PLACEMENT_3D ( 'NONE', #44, #89, #7244 ) ;
#4028 = DIRECTION ( 'NONE',  ( -1.000000000000000000, 1.774937036747276562E-30, 9.447016907875728896E-60 ) ) ;
#4029 = LINE ( 'NONE', #634, #2354 ) ;
#4030 = CIRCLE ( 'NONE', #1395, 0.4000000000000001887 ) ;
#4031 = CARTESIAN_POINT ( 'NONE',  ( 8.000000000000008882, 3.871967595401863083, -7.901061386767627148 ) ) ;
#4032 = CARTESIAN_POINT ( 'NONE',  ( -8.000000000000669687, 0.7809653281580556383, -4.133046444150523246E-13 ) ) ;
#4033 = VERTEX_POINT ( 'NONE', #2503 ) ;
#4034 = VECTOR ( 'NONE', #4767, 1000.000000000000000 ) ;
#4035 = EDGE_CURVE ( 'NONE', #5809, #2338, #1743, .T. ) ;
#4036 = CONICAL_SURFACE ( 'NONE', #1640, 7.000000000000000888, 0.7853981633974482790 ) ;
#4037 = FILL_AREA_STYLE ('',( #818 ) ) ;
#4038 = EDGE_LOOP ( 'NONE', ( #6325, #5378, #3711, #4893 ) ) ;
#4039 = DIRECTION ( 'NONE',  ( 0.000000000000000000, 0.000000000000000000, 1.000000000000000000 ) ) ;
#4040 = AXIS2_PLACEMENT_3D ( 'NONE', #2039, #7347, #7872 ) ;
#4041 = DIRECTION ( 'NONE',  ( 6.400024471206996205E-36, -1.000000000000000000, -7.598173571352216173E-18 ) ) ;
#4042 = MECHANICAL_DESIGN_GEOMETRIC_PRESENTATION_REPRESENTATION (  '', ( #2229 ), #285 ) ;
#4043 = PRODUCT_DEFINITION_SHAPE ( 'NONE', 'NONE',  #7892 ) ;
#4044 = CARTESIAN_POINT ( 'NONE',  ( 275.0000000000000000, -425.0000000000000000, -80.00000000000000000 ) ) ;
#4045 = DIRECTION ( 'NONE',  ( 0.000000000000000000, 0.000000000000000000, -1.000000000000000000 ) ) ;
#4046 = CARTESIAN_POINT ( 'NONE',  ( -8.000000000000225597, 1.572549600175543905, -8.331055444744766447 ) ) ;
#4047 = ORIENTED_EDGE ( 'NONE', *, *, #4048, .F. ) ;
#4048 = EDGE_CURVE ( 'NONE', #1712, #4183, #6599, .T. ) ;
#4049 = ORIENTED_EDGE ( 'NONE', *, *, #1526, .F. ) ;
#4050 = CARTESIAN_POINT ( 'NONE',  ( -74.24999999999971578, 15.00000000000014211, 1.942890293094024198E-13 ) ) ;
#4051 = EDGE_LOOP ( 'NONE', ( #2043, #1581, #2720, #5798 ) ) ;
#4052 = FACE_OUTER_BOUND ( 'NONE', #5336, .T. ) ;
#4053 = CARTESIAN_POINT ( 'NONE',  ( 0.000000000000000000, 0.000000000000000000, -8.400000000000018119 ) ) ;
#4054 = CARTESIAN_POINT ( 'NONE',  ( 0.6527133886630634985, -8.860760056385847960, -0.4969600502618143900 ) ) ;
#4055 = VERTEX_POINT ( 'NONE', #8593 ) ;
#4056 = EDGE_CURVE ( 'NONE', #1742, #3262, #7946, .T. ) ;
#4057 = ORIENTED_EDGE ( 'NONE', *, *, #1268, .T. ) ;
#4058 = EDGE_CURVE ( 'NONE', #2020, #8164, #1036, .T. ) ;
#4059 = ADVANCED_FACE ( 'NONE', ( #898 ), #51, .F. ) ;
#4060 = FACE_OUTER_BOUND ( 'NONE', #5214, .T. ) ;
#4061 = AXIS2_PLACEMENT_3D ( 'NONE', #4323, #6987, #3672 ) ;
#4062 = EDGE_CURVE ( 'NONE', #3453, #1579, #3538, .T. ) ;
#4063 = CYLINDRICAL_SURFACE ( 'NONE', #986, 5.500000000000023981 ) ;
#4064 = ORIENTED_EDGE ( 'NONE', *, *, #6739, .F. ) ;
#4065 = DIRECTION ( 'NONE',  ( -1.000000000000000000, -8.881784197001244435E-16, -0.000000000000000000 ) ) ;
#4066 =( NAMED_UNIT ( * ) PLANE_ANGLE_UNIT ( ) SI_UNIT ( $, .RADIAN. ) );
#4067 = VERTEX_POINT ( 'NONE', #2730 ) ;
#4068 = AXIS2_PLACEMENT_3D ( 'NONE', #5823, #1780, #448 ) ;
#4069 = CARTESIAN_POINT ( 'NONE',  ( -8.000000000000000000, -3.098204225878153917, -0.3157906771918689848 ) ) ;
#4070 = ORIENTED_EDGE ( 'NONE', *, *, #3632, .F. ) ;
#4071 = DIRECTION ( 'NONE',  ( -0.9237280213470678847, -0.3830490080632384942, 0.000000000000000000 ) ) ;
#4072 = CARTESIAN_POINT ( 'NONE',  ( 44.99999999999992895, -500.0000000000000000, 45.00000000000000711 ) ) ;
#4073 = ADVANCED_FACE ( 'NONE', ( #4246, #1538 ), #2123, .T. ) ;
#4074 = DIRECTION ( 'NONE',  ( 0.000000000000000000, 0.000000000000000000, -1.000000000000000000 ) ) ;
#4075 = ORIENTED_EDGE ( 'NONE', *, *, #7376, .T. ) ;
#4076 = CARTESIAN_POINT ( 'NONE',  ( -8.000000000000667910, -3.867591403078892487, -7.902324684675164690 ) ) ;
#4077 = CONICAL_SURFACE ( 'NONE', #5910, 4.057500000000000107, 1.047197551196592746 ) ;
#4078 = AXIS2_PLACEMENT_3D ( 'NONE', #3809, #6466, #5837 ) ;
#4079 = CARTESIAN_POINT ( 'NONE',  ( 5.000000000000115463, 2.342598717236854977, -4.057500000000047180 ) ) ;
#4080 = CARTESIAN_POINT ( 'NONE',  ( -4.000000000000003553, 6.928203230275431501, 0.000000000000000000 ) ) ;
#4081 = DIRECTION ( 'NONE',  ( -1.000000000000000000, -8.881784197001244435E-16, 0.000000000000000000 ) ) ;
#4082 = VERTEX_POINT ( 'NONE', #1419 ) ;
#4083 = FACE_OUTER_BOUND ( 'NONE', #7475, .T. ) ;
#4084 = SURFACE_STYLE_FILL_AREA ( #8 ) ;
#4085 = DIRECTION ( 'NONE',  ( 3.919652622816902408E-30, 3.944304526105059027E-30, -1.000000000000000000 ) ) ;
#4086 = CONICAL_SURFACE ( 'NONE', #5477, 8.000000000000007105, 1.047197551196597631 ) ;
#4087 = AXIS2_PLACEMENT_3D ( 'NONE', #6626, #2787, #5987 ) ;
#4088 = EDGE_CURVE ( 'NONE', #6543, #7164, #7263, .T. ) ;
#4089 = CIRCLE ( 'NONE', #1307, 4.057500000000000107 ) ;
#4090 = FACE_BOUND ( 'NONE', #6071, .T. ) ;
#4091 = LINE ( 'NONE', #6023, #8415 ) ;
#4092 = ORIENTED_EDGE ( 'NONE', *, *, #5327, .F. ) ;
#4093 = FACE_OUTER_BOUND ( 'NONE', #2207, .T. ) ;
#4094 = VERTEX_POINT ( 'NONE', #8038 ) ;
#4095 = CARTESIAN_POINT ( 'NONE',  ( 0.000000000000000000, 0.000000000000000000, 0.000000000000000000 ) ) ;
#4096 = DIRECTION ( 'NONE',  ( -0.000000000000000000, -0.000000000000000000, 1.000000000000000000 ) ) ;
#4097 = DIRECTION ( 'NONE',  ( 1.000000000000000000, 0.000000000000000000, 0.000000000000000000 ) ) ;
#4098 = ADVANCED_FACE ( 'NONE', ( #6909 ), #762, .T. ) ;
#4099 = ORIENTED_EDGE ( 'NONE', *, *, #6939, .F. ) ;
#4100 = DIRECTION ( 'NONE',  ( -3.919652622816902408E-30, -3.944304526105059027E-30, 1.000000000000000000 ) ) ;
#4101 = ORIENTED_EDGE ( 'NONE', *, *, #3461, .F. ) ;
#4102 = AXIS2_PLACEMENT_3D ( 'NONE', #578, #5828, #3837 ) ;
#4103 = EDGE_LOOP ( 'NONE', ( #6344, #6429, #3846, #7003, #8196, #3357 ) ) ;
#4104 = PRODUCT_DEFINITION_SHAPE ( 'NONE', 'NONE',  #8632 ) ;
#4105 = DIRECTION ( 'NONE',  ( 7.420547859534711256E-34, -1.000000000000000000, -1.224646799147352961E-16 ) ) ;
#4106 = ADVANCED_FACE ( 'NONE', ( #937, #5559 ), #3419, .T. ) ;
#4107 = AXIS2_PLACEMENT_3D ( 'NONE', #5898, #1908, #4520 ) ;
#4108 = DIRECTION ( 'NONE',  ( -1.000000000000000000, -8.881784197001244435E-16, 0.000000000000000000 ) ) ;
#4109 = ORIENTED_EDGE ( 'NONE', *, *, #571, .F. ) ;
#4110 = DIRECTION ( 'NONE',  ( 1.000000000000000000, -1.774937036747276562E-30, -9.447016907875728896E-60 ) ) ;
#4111 = CARTESIAN_POINT ( 'NONE',  ( -350.0000000000001137, -2.775557561562891351E-14, 69.99999999999995737 ) ) ;
#4112 = ORIENTED_EDGE ( 'NONE', *, *, #4062, .F. ) ;
#4113 = AXIS2_PLACEMENT_3D ( 'NONE', #8138, #1000, #3654 ) ;
#4114 = ADVANCED_FACE ( 'NONE', ( #7428 ), #2070, .T. ) ;
#4115 = DIRECTION ( 'NONE',  ( 0.000000000000000000, 0.000000000000000000, -1.000000000000000000 ) ) ;
#4116 = PRODUCT_DEFINITION_SHAPE ( 'NONE', 'NONE',  #8609 ) ;
#4117 = EDGE_LOOP ( 'NONE', ( #6609, #7313, #1103 ) ) ;
#4118 = CARTESIAN_POINT ( 'NONE',  ( -8.000000000000007105, -4.618802153517065356, -7.685468820183672278 ) ) ;
#4119 = DIRECTION ( 'NONE',  ( -0.000000000000000000, -0.000000000000000000, 1.000000000000000000 ) ) ;
#4120 = ORIENTED_EDGE ( 'NONE', *, *, #4754, .F. ) ;
#4121 = LINE ( 'NONE', #1587, #7919 ) ;
#4122 = DIRECTION ( 'NONE',  ( 1.000000000000000000, 2.715219353702832714E-15, -4.287287528375070588E-30 ) ) ;
#4123 = DIRECTION ( 'NONE',  ( 1.000000000000000000, 0.000000000000000000, 0.000000000000000000 ) ) ;
#4124 = VERTEX_POINT ( 'NONE', #7555 ) ;
#4125 = CARTESIAN_POINT ( 'NONE',  ( -7.999999999999896083, 3.871967595402032725, -0.4989386132323781475 ) ) ;
#4126 = DIRECTION ( 'NONE',  ( 7.703719777548943412E-34, 0.000000000000000000, -1.000000000000000000 ) ) ;
#4127 =( REPRESENTATION_RELATIONSHIP ('NONE','NONE', #1279, #4003 ) REPRESENTATION_RELATIONSHIP_WITH_TRANSFORMATION ( #1729 )SHAPE_REPRESENTATION_RELATIONSHIP( ) );
#4128 = CARTESIAN_POINT ( 'NONE',  ( -7.347286611336965478, -4.995646404165273502, -0.4969600502617496640 ) ) ;
#4129 = LINE ( 'NONE', #865, #5223 ) ;
#4130 = CARTESIAN_POINT ( 'NONE',  ( 33.00000000000055422, -1.431146867680865853E-14, 6.883382752675970551E-12 ) ) ;
#4131 = PLANE ( 'NONE',  #2372 ) ;
#4132 = VERTEX_POINT ( 'NONE', #233 ) ;
#4133 = AXIS2_PLACEMENT_3D ( 'NONE', #2799, #4630, #2671 ) ;
#4134 = FILL_AREA_STYLE_COLOUR ( '', #701 ) ;
#4135 = ORIENTED_EDGE ( 'NONE', *, *, #6166, .T. ) ;
#4136 = EDGE_CURVE ( 'NONE', #6748, #6426, #457, .T. ) ;
#4137 = CARTESIAN_POINT ( 'NONE',  ( -99.99999999999972999, 0.000000000000000000, -2.775557561562891351E-14 ) ) ;
#4138 = APPLICATION_CONTEXT ( 'automotive_design' ) ;
#4139 = DIRECTION ( 'NONE',  ( 3.851859888774471706E-33, -7.598173571352220795E-18, 1.000000000000000000 ) ) ;
#4140 = DIRECTION ( 'NONE',  ( -1.463706757734299248E-32, 1.000000000000000000, 5.238529448733281520E-32 ) ) ;
#4141 = VERTEX_POINT ( 'NONE', #7382 ) ;
#4142 = VERTEX_POINT ( 'NONE', #4118 ) ;
#4143 = ADVANCED_FACE ( 'NONE', ( #8127 ), #5472, .F. ) ;
#4144 = CIRCLE ( 'NONE', #2759, 15.00000000000000355 ) ;
#4145 = DIRECTION ( 'NONE',  ( -1.000000000000000000, -8.881784197001244435E-16, 0.000000000000000000 ) ) ;
#4146 = ORIENTED_EDGE ( 'NONE', *, *, #6773, .F. ) ;
#4147 = CARTESIAN_POINT ( 'NONE',  ( -3.660532965668796823, 7.124194613927540054, -8.400000000000076739 ) ) ;
#4148 = DIRECTION ( 'NONE',  ( 0.8660254037844369313, 0.5000000000000028866, 0.000000000000000000 ) ) ;
#4149 = CARTESIAN_POINT ( 'NONE',  ( 0.000000000000000000, 0.000000000000000000, 0.000000000000000000 ) ) ;
#4150 = ORIENTED_EDGE ( 'NONE', *, *, #653, .T. ) ;
#4151 = CIRCLE ( 'NONE', #4847, 5.559999999999998721 ) ;
#4152 = EDGE_CURVE ( 'NONE', #7562, #6221, #1497, .T. ) ;
#4153 = ORIENTED_EDGE ( 'NONE', *, *, #7725, .F. ) ;
#4154 = CARTESIAN_POINT ( 'NONE',  ( -44.99999999999992895, -500.0000000000000000, 50.00000000000000000 ) ) ;
#4155 = AXIS2_PLACEMENT_3D ( 'NONE', #7829, #1867, #3216 ) ;
#4156 = DIRECTION ( 'NONE',  ( 6.400024471206993532E-36, -1.000000000000000000, -7.598173571352311699E-18 ) ) ;
#4157 = ORIENTED_EDGE ( 'NONE', *, *, #6583, .T. ) ;
#4158 = B_SPLINE_CURVE_WITH_KNOTS ( 'NONE', 3,
 ( #3142, #2487, #408, #2316, #5746, #5058 ),
 .UNSPECIFIED., .F., .F.,
 ( 4, 2, 4 ),
 ( 2.380731635918682947E-07, 0.002336973833157848703, 0.004673709593152105407 ),
 .UNSPECIFIED. ) ;
#4159 = CARTESIAN_POINT ( 'NONE',  ( 5.355005115540778959, 6.145890662064466881, -0.08224679563958640915 ) ) ;
#4160 = CYLINDRICAL_SURFACE ( 'NONE', #8560, 49.99999999999999289 ) ;
#4161 = ORIENTED_EDGE ( 'NONE', *, *, #952, .F. ) ;
#4162 = EDGE_CURVE ( 'NONE', #872, #7966, #2269, .T. ) ;
#4163 =( NAMED_UNIT ( * ) SI_UNIT ( $, .STERADIAN. ) SOLID_ANGLE_UNIT ( ) );
#4164 = AXIS2_PLACEMENT_3D ( 'NONE', #7422, #6901, #2276 ) ;
#4165 = DIRECTION ( 'NONE',  ( -1.000000000000000000, 1.774937036747276562E-30, 0.000000000000000000 ) ) ;
#4166 = CARTESIAN_POINT ( 'NONE',  ( 4.000000000000003553, -1.759474945355333109, 3.047500000000091802 ) ) ;
#4167 = CARTESIAN_POINT ( 'NONE',  ( 139.9999999999994316, 3.469446951953611664E-14, 4.171999999998556419 ) ) ;
#4168 = AXIS2_PLACEMENT_3D ( 'NONE', #3593, #5602, #267 ) ;
#4169 = CARTESIAN_POINT ( 'NONE',  ( 0.000000000000000000, -299.9999999999999432, -2.775557561562891351E-14 ) ) ;
#4170 = DIRECTION ( 'NONE',  ( -1.000000000000000000, -0.000000000000000000, -0.000000000000000000 ) ) ;
#4171 = ORIENTED_EDGE ( 'NONE', *, *, #5073, .F. ) ;
#4172 = AXIS2_PLACEMENT_3D ( 'NONE', #3976, #3359, #5414 ) ;
#4173 = VERTEX_POINT ( 'NONE', #8167 ) ;
#4174 =( REPRESENTATION_RELATIONSHIP ('NONE','NONE', #1279, #83 ) REPRESENTATION_RELATIONSHIP_WITH_TRANSFORMATION ( #7180 )SHAPE_REPRESENTATION_RELATIONSHIP( ) );
#4175 = CARTESIAN_POINT ( 'NONE',  ( 44.99999999999992895, 425.0000000000000000, -3.122502256758253953E-15 ) ) ;
#4176 = VECTOR ( 'NONE', #3395, 1000.000000000000114 ) ;
#4177 = LINE ( 'NONE', #6848, #1858 ) ;
#4178 = ORIENTED_EDGE ( 'NONE', *, *, #3774, .T. ) ;
#4179 = EDGE_CURVE ( 'NONE', #8044, #5649, #3381, .T. ) ;
#4180 = CARTESIAN_POINT ( 'NONE',  ( 0.000000000000000000, 0.000000000000000000, -8.400000000000018119 ) ) ;
#4181 = VERTEX_POINT ( 'NONE', #7514 ) ;
#4182 = DIRECTION ( 'NONE',  ( 0.000000000000000000, 0.000000000000000000, -1.000000000000000000 ) ) ;
#4183 = VERTEX_POINT ( 'NONE', #2407 ) ;
#4184 = DIRECTION ( 'NONE',  ( 9.447016907875728896E-60, 5.322451846059955323E-30, -1.000000000000000000 ) ) ;
#4185 = CARTESIAN_POINT ( 'NONE',  ( 8.000000000000012434, -0.7805016046295530918, -8.399999999999987921 ) ) ;
#4186 = ADVANCED_FACE ( 'NONE', ( #2281 ), #6576, .T. ) ;
#4187 = EDGE_LOOP ( 'NONE', ( #4641, #3268, #7831, #3961, #1612, #7918 ) ) ;
#4188 = CARTESIAN_POINT ( 'NONE',  ( 1.110223024625156540E-13, 9.237604307033992157, -7.685468820183672278 ) ) ;
#4189 = DIRECTION ( 'NONE',  ( -0.000000000000000000, -0.000000000000000000, 1.000000000000000000 ) ) ;
#4190 = DIRECTION ( 'NONE',  ( 1.000000000000000000, 0.000000000000000000, 0.000000000000000000 ) ) ;
#4191 = ORIENTED_EDGE ( 'NONE', *, *, #1808, .F. ) ;
#4192 = CARTESIAN_POINT ( 'NONE',  ( 0.000000000000000000, -299.9999999999999432, -2.775557561562891351E-14 ) ) ;
#4193 = VERTEX_POINT ( 'NONE', #2573 ) ;
#4194 = CARTESIAN_POINT ( 'NONE',  ( 0.000000000000000000, 295.0000000000000568, -6.938893903907228378E-14 ) ) ;
#4195 = AXIS2_PLACEMENT_3D ( 'NONE', #4731, #1893, #6509 ) ;
#4196 = EDGE_CURVE ( 'NONE', #5835, #698, #1021, .T. ) ;
#4197 = CARTESIAN_POINT ( 'NONE',  ( -8.000000000000229150, 4.618802153516954334, -0.7145311798163467287 ) ) ;
#4198 = ADVANCED_FACE ( 'NONE', ( #2358 ), #3100, .F. ) ;
#4199 = ORIENTED_EDGE ( 'NONE', *, *, #7570, .T. ) ;
#4200 = DIRECTION ( 'NONE',  ( 1.000000000000000000, 0.000000000000000000, -5.478200730701491345E-30 ) ) ;
#4201 = DIRECTION ( 'NONE',  ( -1.774937036747276913E-30, 0.5000000000000014433, 0.8660254037844379305 ) ) ;
#4202 = AXIS2_PLACEMENT_3D ( 'NONE', #7454, #6241, #8342 ) ;
#4203 = CARTESIAN_POINT ( 'NONE',  ( 0.000000000000000000, 0.000000000000000000, 0.000000000000000000 ) ) ;
#4204 = ORIENTED_EDGE ( 'NONE', *, *, #6495, .F. ) ;
#4205 = AXIS2_PLACEMENT_3D ( 'NONE', #1460, #6222, #188 ) ;
#4206 = EDGE_LOOP ( 'NONE', ( #8031, #1889, #6575, #60 ) ) ;
#4207 = FACE_OUTER_BOUND ( 'NONE', #270, .T. ) ;
#4208 = PRODUCT_DEFINITION_CONTEXT ( 'detailed design', #6645, 'design' ) ;
#4209 = VECTOR ( 'NONE', #1920, 1000.000000000000000 ) ;
#4210 = DIRECTION ( 'NONE',  ( 3.919652622816902408E-30, 3.944304526105059027E-30, -1.000000000000000000 ) ) ;
#4211 = VECTOR ( 'NONE', #6202, 1000.000000000000114 ) ;
#4212 = CARTESIAN_POINT ( 'NONE',  ( 0.000000000000000000, 0.000000000000000000, 0.000000000000000000 ) ) ;
#4213 = EDGE_CURVE ( 'NONE', #2938, #4276, #1843, .T. ) ;
#4214 = AXIS2_PLACEMENT_3D ( 'NONE', #3764, #1917, #4574 ) ;
#4215 = DIRECTION ( 'NONE',  ( 1.000000000000000000, -1.774937036747276562E-30, -9.447016907875728896E-60 ) ) ;
#4216 = DIRECTION ( 'NONE',  ( 3.646298014371739284E-59, 1.027162637006519249E-29, -1.000000000000000000 ) ) ;
#4217 = FACE_OUTER_BOUND ( 'NONE', #325, .T. ) ;
#4218 = EDGE_LOOP ( 'NONE', ( #7272, #4714, #7917, #4120, #2274, #5116 ) ) ;
#4219 = FACE_OUTER_BOUND ( 'NONE', #7777, .T. ) ;
#4220 = VERTEX_POINT ( 'NONE', #409 ) ;
#4221 = AXIS2_PLACEMENT_3D ( 'NONE', #2710, #2107, #1313 ) ;
#4222 = AXIS2_PLACEMENT_3D ( 'NONE', #2751, #5409, #7405 ) ;
#4223 = FACE_OUTER_BOUND ( 'NONE', #527, .T. ) ;
#4224 = EDGE_CURVE ( 'NONE', #7660, #3572, #6866, .T. ) ;
#4225 = AXIS2_PLACEMENT_3D ( 'NONE', #1739, #6295, #6451 ) ;
#4226 = AXIS2_PLACEMENT_3D ( 'NONE', #8473, #6438, #476 ) ;
#4227 = CARTESIAN_POINT ( 'NONE',  ( -50.00000000000004263, -425.0000000000000000, -25.00000000000000355 ) ) ;
#4228 = CARTESIAN_POINT ( 'NONE',  ( -2.300000000000024247, 1.224646799147353454E-15, -10.00000000000000178 ) ) ;
#4229 = VERTEX_POINT ( 'NONE', #7681 ) ;
#4230 = DIRECTION ( 'NONE',  ( -1.000000000000000000, -8.881784197001244435E-16, 0.000000000000000000 ) ) ;
#4231 = EDGE_LOOP ( 'NONE', ( #5522, #3728, #1316, #5962 ) ) ;
#4232 = VERTEX_POINT ( 'NONE', #2935 ) ;
#4233 = AXIS2_PLACEMENT_3D ( 'NONE', #5153, #7901, #6643 ) ;
#4234 =( GEOMETRIC_REPRESENTATION_CONTEXT ( 3 ) GLOBAL_UNCERTAINTY_ASSIGNED_CONTEXT ( ( #7167 ) ) GLOBAL_UNIT_ASSIGNED_CONTEXT ( ( #7330, #5421, #1225 ) ) REPRESENTATION_CONTEXT ( 'NONE', 'WORKASPACE' ) );
#4235 = EDGE_CURVE ( 'NONE', #5104, #1055, #5061, .T. ) ;
#4236 = FACE_OUTER_BOUND ( 'NONE', #7497, .T. ) ;
#4237 = AXIS2_PLACEMENT_3D ( 'NONE', #813, #6144, #147 ) ;
#4238 = LINE ( 'NONE', #5741, #5033 ) ;
#4239 = ORIENTED_EDGE ( 'NONE', *, *, #7249, .F. ) ;
#4240 = PLANE ( 'NONE',  #4168 ) ;
#4241 = CARTESIAN_POINT ( 'NONE',  ( -32.49999999999997158, 3.469446951953614189E-15, -6.938893903907228378E-15 ) ) ;
#4242 = DIRECTION ( 'NONE',  ( 1.000000000000000000, -5.898059818321089887E-17, -4.579669976578770729E-16 ) ) ;
#4243 = ORIENTED_EDGE ( 'NONE', *, *, #1505, .T. ) ;
#4244 = DIRECTION ( 'NONE',  ( 1.000000000000000000, 0.000000000000000000, -6.938893903907228378E-17 ) ) ;
#4245 = ORIENTED_EDGE ( 'NONE', *, *, #5145, .T. ) ;
#4246 = FACE_BOUND ( 'NONE', #1160, .T. ) ;
#4247 = ADVANCED_FACE ( 'NONE', ( #7882 ), #3925, .T. ) ;
#4248 = CARTESIAN_POINT ( 'NONE',  ( 3.999999999999337419, -6.928203230275431501, 0.000000000000000000 ) ) ;
#4249 = ORIENTED_EDGE ( 'NONE', *, *, #335, .T. ) ;
#4250 = PRODUCT_DEFINITION_SHAPE ( 'NONE', 'NONE',  #8634 ) ;
#4251 = CARTESIAN_POINT ( 'NONE',  ( 5.690023276062296631, 5.952467836903953646, -0.1306530452036860357 ) ) ;
#4252 = VERTEX_POINT ( 'NONE', #4413 ) ;
#4253 = ORIENTED_EDGE ( 'NONE', *, *, #7521, .F. ) ;
#4254 = EDGE_LOOP ( 'NONE', ( #486, #3260, #4146, #6165 ) ) ;
#4255 = ADVANCED_FACE ( 'NONE', ( #4372 ), #1659, .T. ) ;
#4256 = VECTOR ( 'NONE', #6320, 1000.000000000000000 ) ;
#4257 = DIRECTION ( 'NONE',  ( -0.000000000000000000, -0.000000000000000000, 1.000000000000000000 ) ) ;
#4258 = CARTESIAN_POINT ( 'NONE',  ( 0.000000000000000000, 0.000000000000000000, 0.000000000000000000 ) ) ;
#4259 = DIRECTION ( 'NONE',  ( -1.000000000000000000, 3.549874073494553124E-30, 0.000000000000000000 ) ) ;
#4260 = DIRECTION ( 'NONE',  ( -0.000000000000000000, -0.000000000000000000, 1.000000000000000000 ) ) ;
#4261 = CARTESIAN_POINT ( 'NONE',  ( 1.285879139104721028E-15, 10.50000000000000178, 7.978082249919836843E-17 ) ) ;
#4262 = ORIENTED_EDGE ( 'NONE', *, *, #6314, .T. ) ;
#4263 = CARTESIAN_POINT ( 'NONE',  ( 8.000000000000007105, 4.618802153517065356, -0.7145311798163467287 ) ) ;
#4264 = EDGE_LOOP ( 'NONE', ( #3503, #1143, #50, #8217 ) ) ;
#4265 = EDGE_CURVE ( 'NONE', #4500, #2369, #2957, .T. ) ;
#4266 =( GEOMETRIC_REPRESENTATION_CONTEXT ( 3 ) GLOBAL_UNCERTAINTY_ASSIGNED_CONTEXT ( ( #2346 ) ) GLOBAL_UNIT_ASSIGNED_CONTEXT ( ( #5167, #7870, #3211 ) ) REPRESENTATION_CONTEXT ( 'NONE', 'WORKASPACE' ) );
#4267 = CARTESIAN_POINT ( 'NONE',  ( 4.000000000000003553, 2.639212418032998997, -1.523749999999823856 ) ) ;
#4268 = ORIENTED_EDGE ( 'NONE', *, *, #3709, .F. ) ;
#4269 = CARTESIAN_POINT ( 'NONE',  ( -38.74999999999999289, 4.975595280120367735E-34, 18.00000000000000355 ) ) ;
#4270 = ORIENTED_EDGE ( 'NONE', *, *, #2667, .F. ) ;
#4271 = ORIENTED_EDGE ( 'NONE', *, *, #3346, .F. ) ;
#4272 = EDGE_CURVE ( 'NONE', #1627, #6142, #1333, .T. ) ;
#4273 = EDGE_CURVE ( 'NONE', #7714, #316, #463, .T. ) ;
#4274 = CARTESIAN_POINT ( 'NONE',  ( 2.645508037661955303, 7.710219529346674427, -8.331901280394536258 ) ) ;
#4275 = DIRECTION ( 'NONE',  ( -1.000000000000000000, 3.549874073494553124E-30, 0.000000000000000000 ) ) ;
#4276 = VERTEX_POINT ( 'NONE', #5609 ) ;
#4277 = ADVANCED_FACE ( 'NONE', ( #1066, #8254 ), #6306, .F. ) ;
#4278 = FACE_OUTER_BOUND ( 'NONE', #2066, .T. ) ;
#4279 = DIRECTION ( 'NONE',  ( 1.463706757734299248E-32, -1.000000000000000000, -5.238529448733281520E-32 ) ) ;
#4280 = DIRECTION ( 'NONE',  ( 1.000000000000000000, 8.736544766236844851E-16, -1.058471975245250406E-16 ) ) ;
#4281 = ORIENTED_EDGE ( 'NONE', *, *, #6751, .F. ) ;
#4282 = FACE_BOUND ( 'NONE', #1771, .T. ) ;
#4283 = ORIENTED_EDGE ( 'NONE', *, *, #2339, .T. ) ;
#4284 = DIRECTION ( 'NONE',  ( -1.000000000000000000, 3.549874073494553124E-30, 0.000000000000000000 ) ) ;
#4285 = CARTESIAN_POINT ( 'NONE',  ( 9.999999999999896971, 0.000000000000000000, 0.000000000000000000 ) ) ;
#4286 = DIRECTION ( 'NONE',  ( -3.851859888774471706E-33, 7.598173571352185358E-18, -1.000000000000000000 ) ) ;
#4287 = ORIENTED_EDGE ( 'NONE', *, *, #4995, .T. ) ;
#4288 = AXIS2_PLACEMENT_3D ( 'NONE', #7665, #1682, #4230 ) ;
#4289 = LINE ( 'NONE', #3602, #6266 ) ;
#4290 = PRODUCT_DEFINITION ( 'UNKNOWN', '', #3408, #6551 ) ;
#4291 =( NAMED_UNIT ( * ) SI_UNIT ( $, .STERADIAN. ) SOLID_ANGLE_UNIT ( ) );
#4292 = ORIENTED_EDGE ( 'NONE', *, *, #7389, .T. ) ;
#4293 = DIRECTION ( 'NONE',  ( 0.000000000000000000, 0.000000000000000000, 1.000000000000000000 ) ) ;
#4294 = VERTEX_POINT ( 'NONE', #322 ) ;
#4295 = ORIENTED_EDGE ( 'NONE', *, *, #3632, .T. ) ;
#4296 = DIRECTION ( 'NONE',  ( 1.000000000000000000, -1.774937036747276562E-30, 0.000000000000000000 ) ) ;
#4297 = AXIS2_PLACEMENT_3D ( 'NONE', #6087, #1450, #4108 ) ;
#4298 = CIRCLE ( 'NONE', #1790, 5.499999999999999112 ) ;
#4299 = CARTESIAN_POINT ( 'NONE',  ( 0.000000000000000000, 60.00000000000000000, -50.00000000000000000 ) ) ;
#4300 = DIRECTION ( 'NONE',  ( 0.000000000000000000, 0.000000000000000000, -1.000000000000000000 ) ) ;
#4301 = CARTESIAN_POINT ( 'NONE',  ( 8.000000000000122569, -0.7805016046292545528, -8.399999999999939959 ) ) ;
#4302 = CARTESIAN_POINT ( 'NONE',  ( 8.000000000000007105, 4.618802153516954334, -8.400000000000018119 ) ) ;
#4303 = CARTESIAN_POINT ( 'NONE',  ( 39.75000000000000000, 4.867971026610730028E-15, 16.99999999999991829 ) ) ;
#4304 = ADVANCED_FACE ( 'NONE', ( #8295 ), #5041, .T. ) ;
#4305 = CIRCLE ( 'NONE', #963, 4.057500000000000107 ) ;
#4306 = CARTESIAN_POINT ( 'NONE',  ( 0.000000000000000000, 0.000000000000000000, -8.400000000000018119 ) ) ;
#4307 = ORIENTED_EDGE ( 'NONE', *, *, #1526, .T. ) ;
#4308 = DIRECTION ( 'NONE',  ( 0.000000000000000000, 0.000000000000000000, 1.000000000000000000 ) ) ;
#4309 = ORIENTED_EDGE ( 'NONE', *, *, #343, .F. ) ;
#4310 = CIRCLE ( 'NONE', #5128, 4.250000000000013323 ) ;
#4311 = DIRECTION ( 'NONE',  ( -1.000000000000000000, -8.881784197001244435E-16, 0.000000000000000000 ) ) ;
#4312 = CLOSED_SHELL ( 'NONE', ( #1204, #2408, #7124, #6395, #3061, #4564, #4579, #7024, #2974, #5264, #5278, #7558, #1232, #4790, #4403, #2294, #1112, #2431 ) ) ;
#4313 = DIRECTION ( 'NONE',  ( -1.000000000000000000, 0.000000000000000000, 0.000000000000000000 ) ) ;
#4314 = ORIENTED_EDGE ( 'NONE', *, *, #3573, .F. ) ;
#4315 = EDGE_CURVE ( 'NONE', #7820, #4707, #3683, .T. ) ;
#4316 = CIRCLE ( 'NONE', #5431, 5.500000000000024869 ) ;
#4317 = VECTOR ( 'NONE', #5666, 1000.000000000000000 ) ;
#4318 = VERTEX_POINT ( 'NONE', #6668 ) ;
#4319 = VECTOR ( 'NONE', #4170, 1000.000000000000000 ) ;
#4320 = VECTOR ( 'NONE', #6544, 999.9999999999998863 ) ;
#4321 = CYLINDRICAL_SURFACE ( 'NONE', #4917, 4.250000000000008882 ) ;
#4322 = AXIS2_PLACEMENT_3D ( 'NONE', #2428, #7174, #4469 ) ;
#4323 = CARTESIAN_POINT ( 'NONE',  ( 0.000000000000000000, 9.237604307034130713, -8.400000000000018119 ) ) ;
#4324 = ORIENTED_EDGE ( 'NONE', *, *, #5469, .T. ) ;
#4325 = EDGE_CURVE ( 'NONE', #2703, #2559, #1836, .T. ) ;
#4326 = DIRECTION ( 'NONE',  ( 1.034996974062495067E-32, -0.7071067811865456854, -0.7071067811865493491 ) ) ;
#4327 = ADVANCED_FACE ( 'NONE', ( #788 ), #7273, .T. ) ;
#4328 = DIRECTION ( 'NONE',  ( 0.000000000000000000, 0.000000000000000000, 1.000000000000000000 ) ) ;
#4329 = APPLICATION_PROTOCOL_DEFINITION ( 'draft international standard', 'automotive_design', 1998, #6520 ) ;
#4330 = VERTEX_POINT ( 'NONE', #7455 ) ;
#4331 = CARTESIAN_POINT ( 'NONE',  ( 0.000000000000000000, -1.040834085586084257E-14, -120.0000000000000000 ) ) ;
#4332 = EDGE_LOOP ( 'NONE', ( #7723, #6024, #4944, #2806 ) ) ;
#4333 = DIRECTION ( 'NONE',  ( 3.851859888774471706E-33, -7.598173571352220795E-18, 1.000000000000000000 ) ) ;
#4334 = VECTOR ( 'NONE', #5913, 1000.000000000000000 ) ;
#4335 = CARTESIAN_POINT ( 'NONE',  ( 5.000000000000115463, -14.99999999999990230, 79.99999999999995737 ) ) ;
#4336 = ORIENTED_EDGE ( 'NONE', *, *, #3824, .T. ) ;
#4337 = LINE ( 'NONE', #3843, #4317 ) ;
#4338 = EDGE_LOOP ( 'NONE', ( #3576, #2412, #2118, #5849, #4981 ) ) ;
#4339 = VERTEX_POINT ( 'NONE', #6077 ) ;
#4340 = FACE_OUTER_BOUND ( 'NONE', #1326, .T. ) ;
#4341 = PLANE ( 'NONE',  #7009 ) ;
#4342 = DIRECTION ( 'NONE',  ( 0.000000000000000000, -1.064348848528640405E-29, 1.000000000000000000 ) ) ;
#4343 = CARTESIAN_POINT ( 'NONE',  ( 8.000000000000117240, 4.618802153516954334, -8.400000000000018119 ) ) ;
#4344 = AXIS2_PLACEMENT_3D ( 'NONE', #1958, #3219, #1873 ) ;
#4345 = LINE ( 'NONE', #867, #4477 ) ;
#4346 = LINE ( 'NONE', #7012, #3617 ) ;
#4347 = CARTESIAN_POINT ( 'NONE',  ( 8.000000000000015987, -3.867591403079598589, -0.4976753153247004402 ) ) ;
#4348 = ORIENTED_EDGE ( 'NONE', *, *, #3969, .T. ) ;
#4349 = CARTESIAN_POINT ( 'NONE',  ( 8.000000000000012434, -1.555946510856073273, -0.06708870216335555137 ) ) ;
#4350 = ORIENTED_EDGE ( 'NONE', *, *, #6718, .T. ) ;
#4351 = AXIS2_PLACEMENT_3D ( 'NONE', #2761, #49, #5337 ) ;
#4352 = EDGE_CURVE ( 'NONE', #2597, #2978, #2708, .T. ) ;
#4353 = DIRECTION ( 'NONE',  ( -3.451266460341926211E-31, 0.4999999999999985567, -0.8660254037844393737 ) ) ;
#4354 = ITEM_DEFINED_TRANSFORMATION ( 'NONE', 'NONE', #1861,  #7563 ) ;
#4355 = CARTESIAN_POINT ( 'NONE',  ( -31.74999999999994316, 0.000000000000000000, 0.000000000000000000 ) ) ;
#4356 = ORIENTED_EDGE ( 'NONE', *, *, #3136, .F. ) ;
#4357 = CIRCLE ( 'NONE', #7142, 5.559999999999998721 ) ;
#4358 = VERTEX_POINT ( 'NONE', #8571 ) ;
#4359 = DIRECTION ( 'NONE',  ( 0.000000000000000000, 0.000000000000000000, -1.000000000000000000 ) ) ;
#4360 = VECTOR ( 'NONE', #4709, 1000.000000000000000 ) ;
#4361 = AXIS2_PLACEMENT_3D ( 'NONE', #5258, #6611, #3294 ) ;
#4362 = EDGE_CURVE ( 'NONE', #7027, #1769, #5268, .T. ) ;
#4363 = UNCERTAINTY_MEASURE_WITH_UNIT (LENGTH_MEASURE( 1.000000000000000082E-05 ), #6312, 'distance_accuracy_value', 'NONE');
#4364 = LINE ( 'NONE', #3714, #36 ) ;
#4365 = CARTESIAN_POINT ( 'NONE',  ( -8.000000000000229150, 4.440892098500626162E-13, -8.400000000000018119 ) ) ;
#4366 = CARTESIAN_POINT ( 'NONE',  ( 7.347286611336940609, 4.995646404165252186, -0.4969600502617288473 ) ) ;
#4367 = ORIENTED_EDGE ( 'NONE', *, *, #6937, .F. ) ;
#4368 = DIRECTION ( 'NONE',  ( -1.000000000000000000, -8.881784197001244435E-16, 0.000000000000000000 ) ) ;
#4369 = CARTESIAN_POINT ( 'NONE',  ( 3.319543390095480717, -7.321065037175468859, -8.383111142572358787 ) ) ;
#4370 = APPLICATION_PROTOCOL_DEFINITION ( 'draft international standard', 'automotive_design', 1998, #6215 ) ;
#4371 = DIRECTION ( 'NONE',  ( -1.000000000000000000, 1.774937036747276562E-30, 0.000000000000000000 ) ) ;
#4372 = FACE_OUTER_BOUND ( 'NONE', #3364, .T. ) ;
#4373 = AXIS2_PLACEMENT_3D ( 'NONE', #315, #3638, #849 ) ;
#4374 = EDGE_CURVE ( 'NONE', #4132, #2959, #4643, .T. ) ;
#4375 = EDGE_CURVE ( 'NONE', #3380, #3572, #4796, .T. ) ;
#4376 = CYLINDRICAL_SURFACE ( 'NONE', #8459, 5.500000000000000000 ) ;
#4377 = ORIENTED_EDGE ( 'NONE', *, *, #6246, .F. ) ;
#4378 = DIRECTION ( 'NONE',  ( -1.000000000000000000, 1.774937036747276562E-30, 0.000000000000000000 ) ) ;
#4379 = PRODUCT_DEFINITION_FORMATION_WITH_SPECIFIED_SOURCE ( 'ANY', '', #6615, .NOT_KNOWN. ) ;
#4380 = SHAPE_REPRESENTATION_RELATIONSHIP ( 'NONE' , 'NONE' ,  #83, #6359 ) ;
#4381 = ORIENTED_EDGE ( 'NONE', *, *, #2217, .F. ) ;
#4382 = ORIENTED_EDGE ( 'NONE', *, *, #8030, .F. ) ;
#4383 = CARTESIAN_POINT ( 'NONE',  ( 5.355005115540780736, 6.145890662064464216, -8.317753204360434083 ) ) ;
#4384 = PRODUCT_DEFINITION_SHAPE ( 'NONE', 'NONE',  #3118 ) ;
#4385 = ORIENTED_EDGE ( 'NONE', *, *, #3069, .F. ) ;
#4386 = B_SPLINE_CURVE_WITH_KNOTS ( 'NONE', 3,
 ( #2826, #5451, #2092, #7396, #7156, #17, #1178, #2700 ),
 .UNSPECIFIED., .F., .F.,
 ( 4, 2, 2, 4 ),
 ( 0.004673709593151625756, 0.005837709341827238343, 0.007001709090502850064, 0.009329708587854075238 ),
 .UNSPECIFIED. ) ;
#4387 = CARTESIAN_POINT ( 'NONE',  ( 0.000000000000000000, 32.50000000000005684, 18.00000000000000355 ) ) ;
#4388 = EDGE_CURVE ( 'NONE', #5867, #4837, #3966, .T. ) ;
#4389 = DIRECTION ( 'NONE',  ( 1.000000000000000000, 3.083952846180997183E-15, -4.108650548026112028E-30 ) ) ;
#4390 = CIRCLE ( 'NONE', #7851, 4.057500000000000107 ) ;
#4391 = DIRECTION ( 'NONE',  ( -3.851859888774471706E-33, -1.232595164407830946E-32, -1.000000000000000000 ) ) ;
#4392 = CARTESIAN_POINT ( 'NONE',  ( -49.99999999999944578, 152.5000000000003126, 9.999999999999786837 ) ) ;
#4393 = AXIS2_PLACEMENT_3D ( 'NONE', #3853, #3899, #4201 ) ;
#4394 = CARTESIAN_POINT ( 'NONE',  ( 8.000000000000012434, -0.7805016046290643716, -8.400000000000012790 ) ) ;
#4395 = EDGE_LOOP ( 'NONE', ( #2298, #6267, #1776 ) ) ;
#4396 = PRODUCT_DEFINITION_SHAPE ( 'NONE', 'NONE',  #8629 ) ;
#4397 = FACE_OUTER_BOUND ( 'NONE', #3582, .T. ) ;
#4398 = ORIENTED_EDGE ( 'NONE', *, *, #1161, .T. ) ;
#4399 = DIRECTION ( 'NONE',  ( 0.000000000000000000, 0.000000000000000000, 1.000000000000000000 ) ) ;
#4400 = DIRECTION ( 'NONE',  ( 4.622231866529366047E-33, -1.224646799147353454E-16, 1.000000000000000000 ) ) ;
#4401 = VERTEX_POINT ( 'NONE', #3913 ) ;
#4402 = DIRECTION ( 'NONE',  ( 0.000000000000000000, 0.000000000000000000, -1.000000000000000000 ) ) ;
#4403 = ADVANCED_FACE ( 'NONE', ( #656 ), #480, .T. ) ;
#4404 = EDGE_CURVE ( 'NONE', #3409, #2313, #4867, .T. ) ;
#4405=STYLED_ITEM('',(#8649),#5730);
#4406 = FACE_OUTER_BOUND ( 'NONE', #3604, .T. ) ;
#4407 = DIRECTION ( 'NONE',  ( -1.000000000000000000, -0.000000000000000000, -0.000000000000000000 ) ) ;
#4408 = ORIENTED_EDGE ( 'NONE', *, *, #899, .T. ) ;
#4409 = DIRECTION ( 'NONE',  ( 0.000000000000000000, 0.000000000000000000, 1.000000000000000000 ) ) ;
#4410 = ADVANCED_FACE ( 'NONE', ( #2749 ), #26, .F. ) ;
#4411 = CARTESIAN_POINT ( 'NONE',  ( -39.75000000000000000, -1.165861408448480429E-31, 16.99999999999991829 ) ) ;
#4412 = AXIS2_PLACEMENT_3D ( 'NONE', #4053, #6670, #8148 ) ;
#4413 = CARTESIAN_POINT ( 'NONE',  ( -25.74999999999986855, 15.00000000000010836, -2.234078735489214329E-29 ) ) ;
#4414 =( REPRESENTATION_RELATIONSHIP ('NONE','NONE', #1279, #83 ) REPRESENTATION_RELATIONSHIP_WITH_TRANSFORMATION ( #1865 )SHAPE_REPRESENTATION_RELATIONSHIP( ) );
#4415 = CARTESIAN_POINT ( 'NONE',  ( 1.285879139104722211E-15, 10.50000000000000711, 130.0000000000000000 ) ) ;
#4416 = ORIENTED_EDGE ( 'NONE', *, *, #7757, .F. ) ;
#4417 = DIRECTION ( 'NONE',  ( 3.919652622816902408E-30, 3.944304526105059027E-30, -1.000000000000000000 ) ) ;
#4418 = EDGE_CURVE ( 'NONE', #3844, #5776, #5364, .T. ) ;
#4419 = ORIENTED_EDGE ( 'NONE', *, *, #8048, .F. ) ;
#4420 = CARTESIAN_POINT ( 'NONE',  ( 1.313474075706797528, 8.479269695851089139, -0.3167204509599274576 ) ) ;
#4421 = ORIENTED_EDGE ( 'NONE', *, *, #8140, .T. ) ;
#4422 = CARTESIAN_POINT ( 'NONE',  ( 2.645508037661961520, 7.710219529346607814, -8.331901280394573561 ) ) ;
#4423 = DIRECTION ( 'NONE',  ( -1.000000000000000000, -0.000000000000000000, -0.000000000000000000 ) ) ;
#4424 = EDGE_CURVE ( 'NONE', #4437, #6290, #5319, .T. ) ;
#4425 = PLANE ( 'NONE',  #7545 ) ;
#4426 = CARTESIAN_POINT ( 'NONE',  ( 4.000000000000114575, 6.928203230275597591, 0.000000000000000000 ) ) ;
#4427 = EDGE_CURVE ( 'NONE', #2167, #7175, #8528, .T. ) ;
#4428 = CARTESIAN_POINT ( 'NONE',  ( 275.0000000000000000, -425.0000000000000000, -80.00000000000000000 ) ) ;
#4429 = VERTEX_POINT ( 'NONE', #5206 ) ;
#4430 = ORIENTED_EDGE ( 'NONE', *, *, #2260, .F. ) ;
#4431 = EDGE_CURVE ( 'NONE', #7587, #18, #2662, .T. ) ;
#4432 = DIRECTION ( 'NONE',  ( 0.000000000000000000, -5.322451846059955323E-30, 1.000000000000000000 ) ) ;
#4433 = AXIS2_PLACEMENT_3D ( 'NONE', #5084, #5773, #7099 ) ;
#4434 = EDGE_CURVE ( 'NONE', #3744, #5809, #1703, .T. ) ;
#4435 = AXIS2_PLACEMENT_3D ( 'NONE', #8372, #4275, #2399 ) ;
#4436 = CARTESIAN_POINT ( 'NONE',  ( -50.00000000000004263, 425.0000000000000000, -25.00000000000000355 ) ) ;
#4437 = VERTEX_POINT ( 'NONE', #1352 ) ;
#4438 = CONICAL_SURFACE ( 'NONE', #5567, 8.000000000000007105, 1.047197551196597631 ) ;
#4439 = CIRCLE ( 'NONE', #265, 4.499999999999990230 ) ;
#4440 = EDGE_CURVE ( 'NONE', #3768, #988, #8019, .T. ) ;
#4441 = CARTESIAN_POINT ( 'NONE',  ( -8.000000000000229150, 4.618802153516954334, -7.685468820183672278 ) ) ;
#4442 = VECTOR ( 'NONE', #5972, 1000.000000000000000 ) ;
#4443 = FACE_OUTER_BOUND ( 'NONE', #5817, .T. ) ;
#4444 = DIRECTION ( 'NONE',  ( 1.000000000000000000, -1.774937036747276562E-30, 0.000000000000000000 ) ) ;
#4445 = ORIENTED_EDGE ( 'NONE', *, *, #1328, .F. ) ;
#4446 = B_SPLINE_CURVE_WITH_KNOTS ( 'NONE', 3,
 ( #7248, #1282, #5340, #7995, #1230, #4026, #5926, #584 ),
 .UNSPECIFIED., .F., .F.,
 ( 4, 2, 2, 4 ),
 ( 0.004673709593152344799, 0.005837709341827777842, 0.007001709090503210886, 0.009329708587854076973 ),
 .UNSPECIFIED. ) ;
#4447 = CARTESIAN_POINT ( 'NONE',  ( 5.000000000000004441, 4.685197434473897360, 0.000000000000000000 ) ) ;
#4448 = AXIS2_PLACEMENT_3D ( 'NONE', #5921, #3979, #1456 ) ;
#4449 = AXIS2_PLACEMENT_3D ( 'NONE', #3761, #6420, #453 ) ;
#4450 = CARTESIAN_POINT ( 'NONE',  ( 4.000000000000003553, -6.928203230275542523, -8.400000000000018119 ) ) ;
#4451 = CARTESIAN_POINT ( 'NONE',  ( 1.310872448937506096, -8.480771745766409353, -8.082649155111401029 ) ) ;
#4452 = PRODUCT_CONTEXT ( 'NONE', #6868, 'mechanical' ) ;
#4453 = AXIS2_PLACEMENT_3D ( 'NONE', #3589, #968, #6250 ) ;
#4454 = ADVANCED_FACE ( 'NONE', ( #4052, #3951 ), #1904, .T. ) ;
#4455 = DIRECTION ( 'NONE',  ( -0.000000000000000000, -0.000000000000000000, 1.000000000000000000 ) ) ;
#4456 = EDGE_LOOP ( 'NONE', ( #3718, #8082, #8564, #3220 ) ) ;
#4457 = CYLINDRICAL_SURFACE ( 'NONE', #4864, 4.499999999999997335 ) ;
#4458 = ORIENTED_EDGE ( 'NONE', *, *, #8274, .T. ) ;
#4459 = CARTESIAN_POINT ( 'NONE',  ( -0.6527133886628254666, 8.860760056385792893, -0.4969600502617717019 ) ) ;
#4460 = ORIENTED_EDGE ( 'NONE', *, *, #3994, .F. ) ;
#4461 = CARTESIAN_POINT ( 'NONE',  ( 1.110223024625156540E-13, 9.237604307033992157, -7.685468820183672278 ) ) ;
#4462 = ADVANCED_FACE ( 'NONE', ( #600 ), #2600, .T. ) ;
#4463 = B_SPLINE_CURVE_WITH_KNOTS ( 'NONE', 3,
 ( #1477, #160, #871, #4793, #7452, #6664 ),
 .UNSPECIFIED., .F., .F.,
 ( 4, 2, 4 ),
 ( 0.008240550023493657672, 0.01057684187039431394, 0.01291313371729497020 ),
 .UNSPECIFIED. ) ;
#4464 = DIRECTION ( 'NONE',  ( 0.5000000000000029976, -0.8660254037844370423, 0.000000000000000000 ) ) ;
#4465 = DIRECTION ( 'NONE',  ( -7.703719777548943412E-34, 0.000000000000000000, 1.000000000000000000 ) ) ;
#4466 = CARTESIAN_POINT ( 'NONE',  ( -4.000000000000003553, -6.928203230275431501, 0.000000000000000000 ) ) ;
#4467 = DIRECTION ( 'NONE',  ( 1.000000000000000000, -0.000000000000000000, -6.938893903907228378E-17 ) ) ;
#4468 = DIRECTION ( 'NONE',  ( -1.000000000000000000, 3.549874073494553124E-30, 0.000000000000000000 ) ) ;
#4469 = DIRECTION ( 'NONE',  ( -1.000000000000000000, -8.881784197001244435E-16, 0.000000000000000000 ) ) ;
#4470 = ORIENTED_EDGE ( 'NONE', *, *, #386, .T. ) ;
#4471 = EDGE_CURVE ( 'NONE', #3196, #6090, #1182, .T. ) ;
#4472 = DIRECTION ( 'NONE',  ( -1.000000000000000000, -8.881784197001244435E-16, 0.000000000000000000 ) ) ;
#4473 = EDGE_CURVE ( 'NONE', #7471, #4915, #5339, .T. ) ;
#4474 = DIRECTION ( 'NONE',  ( 0.000000000000000000, 0.4999999999999986677, -0.8660254037844393737 ) ) ;
#4475 = ORIENTED_EDGE ( 'NONE', *, *, #4780, .F. ) ;
#4476 = VERTEX_POINT ( 'NONE', #7935 ) ;
#4477 = VECTOR ( 'NONE', #6277, 999.9999999999998863 ) ;
#4478 = DIRECTION ( 'NONE',  ( 1.000000000000000000, 0.000000000000000000, 0.000000000000000000 ) ) ;
#4479 = VERTEX_POINT ( 'NONE', #622 ) ;
#4480 = EDGE_CURVE ( 'NONE', #683, #4429, #3839, .T. ) ;
#4481 = VECTOR ( 'NONE', #5757, 1000.000000000000227 ) ;
#4482 = FACE_BOUND ( 'NONE', #2248, .T. ) ;
#4483 = DIRECTION ( 'NONE',  ( -1.463706757734299248E-32, 1.000000000000000000, 5.238529448733281520E-32 ) ) ;
#4484 = AXIS2_PLACEMENT_3D ( 'NONE', #904, #760, #4771 ) ;
#4485 = LINE ( 'NONE', #5230, #304 ) ;
#4486 = FILL_AREA_STYLE ('',( #7796 ) ) ;
#4487 = ORIENTED_EDGE ( 'NONE', *, *, #7801, .F. ) ;
#4488 = FACE_OUTER_BOUND ( 'NONE', #6418, .T. ) ;
#4489 = AXIS2_PLACEMENT_3D ( 'NONE', #2982, #6385, #5018 ) ;
#4490 = DIRECTION ( 'NONE',  ( -1.000000000000000000, -2.715219353702835870E-15, 0.000000000000000000 ) ) ;
#4491 = CARTESIAN_POINT ( 'NONE',  ( 3.999999999999337419, -6.928203230275431501, -8.400000000000018119 ) ) ;
#4492 = DIRECTION ( 'NONE',  ( 1.000000000000000000, 8.736544766236848795E-16, -1.058471975245254351E-16 ) ) ;
#4493 = CARTESIAN_POINT ( 'NONE',  ( 0.000000000000000000, 0.000000000000000000, 0.000000000000000000 ) ) ;
#4494 = AXIS2_PLACEMENT_3D ( 'NONE', #6086, #82, #798 ) ;
#4495 = CARTESIAN_POINT ( 'NONE',  ( 275.0000000000000000, -425.0000000000000000, -75.00000000000000000 ) ) ;
#4496 = VERTEX_POINT ( 'NONE', #7894 ) ;
#4497 = CARTESIAN_POINT ( 'NONE',  ( -31.74999999999994316, -1.972152263052529514E-28, 0.000000000000000000 ) ) ;
#4498 = FACE_OUTER_BOUND ( 'NONE', #1946, .T. ) ;
#4499 =( NAMED_UNIT ( * ) PLANE_ANGLE_UNIT ( ) SI_UNIT ( $, .RADIAN. ) );
#4500 = VERTEX_POINT ( 'NONE', #1269 ) ;
#4501 = EDGE_CURVE ( 'NONE', #5698, #3548, #3924, .T. ) ;
#4502 =( GEOMETRIC_REPRESENTATION_CONTEXT ( 3 ) GLOBAL_UNCERTAINTY_ASSIGNED_CONTEXT ( ( #8559 ) ) GLOBAL_UNIT_ASSIGNED_CONTEXT ( ( #7989, #4066, #5922 ) ) REPRESENTATION_CONTEXT ( 'NONE', 'WORKASPACE' ) );
#4503 = DIRECTION ( 'NONE',  ( -1.000000000000000000, -2.824407374646398239E-13, 0.000000000000000000 ) ) ;
#4504 = ORIENTED_EDGE ( 'NONE', *, *, #964, .F. ) ;
#4505 = PLANE ( 'NONE',  #4233 ) ;
#4506 = CARTESIAN_POINT ( 'NONE',  ( 0.000000000000000000, 5.559999999999995168, 0.000000000000000000 ) ) ;
#4507 = LINE ( 'NONE', #7010, #1609 ) ;
#4508 = PRODUCT_DEFINITION_FORMATION_WITH_SPECIFIED_SOURCE ( 'ANY', '', #8343, .NOT_KNOWN. ) ;
#4509 = CARTESIAN_POINT ( 'NONE',  ( -2.300000000000024247, 0.000000000000000000, 0.000000000000000000 ) ) ;
#4510 = DIRECTION ( 'NONE',  ( -1.463706757734299248E-32, 1.000000000000000000, 5.238529448733281520E-32 ) ) ;
#4511 = LINE ( 'NONE', #681, #7588 ) ;
#4512 = EDGE_CURVE ( 'NONE', #21, #5689, #5049, .T. ) ;
#4513 = CARTESIAN_POINT ( 'NONE',  ( 7.999999999999340972, -4.618802153516732290, -0.7145311798163467287 ) ) ;
#4514 = ORIENTED_EDGE ( 'NONE', *, *, #7719, .F. ) ;
#4515 = ADVANCED_FACE ( 'NONE', ( #5461 ), #6897, .T. ) ;
#4516 = CONICAL_SURFACE ( 'NONE', #763, 8.000000000000007105, 1.047197551196597631 ) ;
#4517 = ORIENTED_EDGE ( 'NONE', *, *, #2178, .F. ) ;
#4518 = DIRECTION ( 'NONE',  ( 1.000000000000000000, 2.715219353702832714E-15, -4.287287528375070588E-30 ) ) ;
#4519 = PRODUCT_DEFINITION_SHAPE ( 'NONE', 'NONE',  #944 ) ;
#4520 = DIRECTION ( 'NONE',  ( -7.703719777548943412E-34, 0.000000000000000000, 1.000000000000000000 ) ) ;
#4521 = CIRCLE ( 'NONE', #8421, 4.250000000000010658 ) ;
#4522 = CONTEXT_DEPENDENT_SHAPE_REPRESENTATION ( #4569, #8358 ) ;
#4523 = ORIENTED_EDGE ( 'NONE', *, *, #5859, .F. ) ;
#4524 = LINE ( 'NONE', #4436, #1091 ) ;
#4525 = EDGE_LOOP ( 'NONE', ( #3782, #2796 ) ) ;
#4526 = EDGE_LOOP ( 'NONE', ( #5063, #5971, #438, #7847 ) ) ;
#4527 = CARTESIAN_POINT ( 'NONE',  ( 0.000000000000000000, -32.50000000000004974, 0.000000000000000000 ) ) ;
#4528 = EDGE_CURVE ( 'NONE', #3289, #5471, #6188, .T. ) ;
#4529 = ORIENTED_EDGE ( 'NONE', *, *, #4235, .F. ) ;
#4530 = CARTESIAN_POINT ( 'NONE',  ( 5.000000000000115463, 2.342598717236854977, -4.057500000000047180 ) ) ;
#4531 = FACE_OUTER_BOUND ( 'NONE', #1935, .T. ) ;
#4532 = DIRECTION ( 'NONE',  ( -1.000000000000000000, 2.842664852890546338E-35, 1.540743955509788340E-33 ) ) ;
#4533 = B_SPLINE_CURVE_WITH_KNOTS ( 'NONE', 3,
 ( #1385, #3213, #4746, #64, #7392, #6754 ),
 .UNSPECIFIED., .F., .F.,
 ( 4, 2, 4 ),
 ( 2.380731632860738630E-07, 0.002336973833158035620, 0.004673709593152784551 ),
 .UNSPECIFIED. ) ;
#4534 = CARTESIAN_POINT ( 'NONE',  ( 275.0000000000000000, -425.0000000000000000, 0.000000000000000000 ) ) ;
#4535 = DIRECTION ( 'NONE',  ( 0.000000000000000000, 0.000000000000000000, 1.000000000000000000 ) ) ;
#4536 = VERTEX_POINT ( 'NONE', #2227 ) ;
#4537 = FACE_OUTER_BOUND ( 'NONE', #1463, .T. ) ;
#4538 = SHAPE_DEFINITION_REPRESENTATION ( #3058, #83 ) ;
#4539 = AXIS2_PLACEMENT_3D ( 'NONE', #4212, #3519, #5673 ) ;
#4540 = VECTOR ( 'NONE', #1382, 1000.000000000000000 ) ;
#4541 = LINE ( 'NONE', #7199, #3871 ) ;
#4542 = ORIENTED_EDGE ( 'NONE', *, *, #1302, .F. ) ;
#4543 = DIRECTION ( 'NONE',  ( 0.000000000000000000, 0.000000000000000000, -1.000000000000000000 ) ) ;
#4544 =( LENGTH_UNIT ( ) NAMED_UNIT ( * ) SI_UNIT ( .MILLI., .METRE. ) );
#4545 = VERTEX_POINT ( 'NONE', #7544 ) ;
#4546 = DIRECTION ( 'NONE',  ( -7.420547859534711256E-34, 1.000000000000000000, 1.224646799147352961E-16 ) ) ;
#4547 = EDGE_LOOP ( 'NONE', ( #923, #1530, #5754, #5422 ) ) ;
#4548 = CARTESIAN_POINT ( 'NONE',  ( 44.99999999999992895, 500.0000000000000000, -45.00000000000000711 ) ) ;
#4549 = EDGE_CURVE ( 'NONE', #4883, #6497, #1569, .T. ) ;
#4550 = LINE ( 'NONE', #3894, #7883 ) ;
#4551 = PRODUCT_DEFINITION ( 'UNKNOWN', '', #488, #5154 ) ;
#4552 = CARTESIAN_POINT ( 'NONE',  ( 0.000000000000000000, 0.000000000000000000, 10.00000000000000888 ) ) ;
#4553 = CARTESIAN_POINT ( 'NONE',  ( 9.184850993605156622E-15, -294.9999999999998295, -75.00000000000008527 ) ) ;
#4554 = PLANE ( 'NONE',  #2091 ) ;
#4555 = DIRECTION ( 'NONE',  ( 3.821045009664296251E-30, -3.944304526105037307E-30, 1.000000000000000000 ) ) ;
#4556 = DIRECTION ( 'NONE',  ( -3.851859888774471706E-33, -1.232595164407830946E-32, -1.000000000000000000 ) ) ;
#4557 = ORIENTED_EDGE ( 'NONE', *, *, #3792, .T. ) ;
#4558 = VERTEX_POINT ( 'NONE', #925 ) ;
#4559 = CARTESIAN_POINT ( 'NONE',  ( 0.000000000000000000, 0.000000000000000000, -8.400000000000018119 ) ) ;
#4560 = DIRECTION ( 'NONE',  ( 0.000000000000000000, 1.000000000000000000, 0.000000000000000000 ) ) ;
#4561 = DIRECTION ( 'NONE',  ( 1.000000000000000000, 0.000000000000000000, 0.000000000000000000 ) ) ;
#4562 = CARTESIAN_POINT ( 'NONE',  ( 0.000000000000000000, 0.000000000000000000, 18.00000000000000355 ) ) ;
#4563 = PLANE ( 'NONE',  #5671 ) ;
#4564 = ADVANCED_FACE ( 'NONE', ( #1528 ), #1490, .T. ) ;
#4565 = VERTEX_POINT ( 'NONE', #6212 ) ;
#4566 = FACE_OUTER_BOUND ( 'NONE', #1887, .T. ) ;
#4567 = AXIS2_PLACEMENT_3D ( 'NONE', #6332, #5688, #4313 ) ;
#4568 = ORIENTED_EDGE ( 'NONE', *, *, #3608, .T. ) ;
#4569 =( REPRESENTATION_RELATIONSHIP ('NONE','NONE', #1279, #4003 ) REPRESENTATION_RELATIONSHIP_WITH_TRANSFORMATION ( #1086 )SHAPE_REPRESENTATION_RELATIONSHIP( ) );
#4570 = ORIENTED_EDGE ( 'NONE', *, *, #8586, .T. ) ;
#4571 = DIRECTION ( 'NONE',  ( -7.703719777548943412E-34, 0.000000000000000000, 1.000000000000000000 ) ) ;
#4572 = EDGE_LOOP ( 'NONE', ( #1684, #1135, #4681, #8189 ) ) ;
#4573 = AXIS2_PLACEMENT_3D ( 'NONE', #8312, #3702, #6281 ) ;
#4574 = DIRECTION ( 'NONE',  ( 6.400024471206997542E-36, -1.000000000000000000, 0.000000000000000000 ) ) ;
#4575 = AXIS2_PLACEMENT_3D ( 'NONE', #6445, #7744, #483 ) ;
#4576 = DIRECTION ( 'NONE',  ( 4.622231866529366732E-33, -1.224646799147352961E-16, 1.000000000000000000 ) ) ;
#4577 = AXIS2_PLACEMENT_3D ( 'NONE', #2492, #1705, #1793 ) ;
#4578 = CARTESIAN_POINT ( 'NONE',  ( 0.000000000000000000, 0.000000000000000000, 0.000000000000000000 ) ) ;
#4579 = ADVANCED_FACE ( 'NONE', ( #4236 ), #884, .T. ) ;
#4580 = DIRECTION ( 'NONE',  ( -1.000000000000000000, -8.881784197001244435E-16, 0.000000000000000000 ) ) ;
#4581 = SURFACE_SIDE_STYLE ('',( #7840 ) ) ;
#4582 = ORIENTED_EDGE ( 'NONE', *, *, #1266, .F. ) ;
#4583 = DIRECTION ( 'NONE',  ( 1.000000000000000000, 0.000000000000000000, 0.000000000000000000 ) ) ;
#4584 = CONTEXT_DEPENDENT_SHAPE_REPRESENTATION ( #1735, #2112 ) ;
#4585 = CONICAL_SURFACE ( 'NONE', #2635, 8.000000000000007105, 1.047197551196597631 ) ;
#4586 = ADVANCED_BREP_SHAPE_REPRESENTATION ( '', ( #40, #7563 ), #7435 ) ;
#4587 = CONICAL_SURFACE ( 'NONE', #2094, 8.000000000000007105, 1.047197551196597631 ) ;
#4588 = ADVANCED_FACE ( 'NONE', ( #4807 ), #7463, .F. ) ;
#4589 = CARTESIAN_POINT ( 'NONE',  ( 4.000000000000058620, 3.518949890710762585, 2.220446049250313081E-13 ) ) ;
#4590 = ORIENTED_EDGE ( 'NONE', *, *, #296, .F. ) ;
#4591 = ADVANCED_FACE ( 'NONE', ( #4060 ), #3936, .F. ) ;
#4592 = DIRECTION ( 'NONE',  ( -3.851859888774471706E-33, -1.232595164407830946E-32, -1.000000000000000000 ) ) ;
#4593 = AXIS2_PLACEMENT_3D ( 'NONE', #5850, #8477, #3858 ) ;
#4594 = ORIENTED_EDGE ( 'NONE', *, *, #1173, .F. ) ;
#4595 = ADVANCED_FACE ( 'NONE', ( #5415 ), #1571, .T. ) ;
#4596 = CARTESIAN_POINT ( 'NONE',  ( -8.000000000000007105, 4.618802153517009401, -0.7145311798163467287 ) ) ;
#4597 = ORIENTED_EDGE ( 'NONE', *, *, #1912, .T. ) ;
#4598 = DIRECTION ( 'NONE',  ( 1.000000000000000000, 3.083952846180992055E-15, -5.478200730701473829E-30 ) ) ;
#4599 = AXIS2_PLACEMENT_3D ( 'NONE', #2616, #3971, #3311 ) ;
#4600 = DIRECTION ( 'NONE',  ( 0.000000000000000000, 0.000000000000000000, 1.000000000000000000 ) ) ;
#4601 = DIRECTION ( 'NONE',  ( 1.000000000000000000, 0.000000000000000000, 0.000000000000000000 ) ) ;
#4602 = FACE_OUTER_BOUND ( 'NONE', #4839, .T. ) ;
#4603 = SHAPE_REPRESENTATION ( 'Rectangular section tube 100x100x5', ( #7563 ), #3529 ) ;
#4604 = CARTESIAN_POINT ( 'NONE',  ( 0.000000000000000000, 6.066788436613252661E-29, -5.700000000000001954 ) ) ;
#4605 = CARTESIAN_POINT ( 'NONE',  ( 275.0000000000000000, 425.0000000000000000, 1.561424668912875158E-13 ) ) ;
#4606 = EDGE_LOOP ( 'NONE', ( #6823, #8173, #5545, #7431 ) ) ;
#4607 = AXIS2_PLACEMENT_3D ( 'NONE', #340, #7653, #8310 ) ;
#4608 = FACE_OUTER_BOUND ( 'NONE', #3169, .T. ) ;
#4609 = ORIENTED_EDGE ( 'NONE', *, *, #3570, .T. ) ;
#4610 = CARTESIAN_POINT ( 'NONE',  ( 4.000000000000003553, 1.759474945355374409, 3.047499999999869758 ) ) ;
#4611 = CARTESIAN_POINT ( 'NONE',  ( -8.000000000000007105, 0.000000000000000000, 0.000000000000000000 ) ) ;
#4612 = CARTESIAN_POINT ( 'NONE',  ( -0.6543471694412738016, -8.859816792613717240, -0.4964154566688340764 ) ) ;
#4613 = CARTESIAN_POINT ( 'NONE',  ( 0.000000000000000000, 0.000000000000000000, -109.9999999999999574 ) ) ;
#4614 = ORIENTED_EDGE ( 'NONE', *, *, #2155, .F. ) ;
#4615 = CARTESIAN_POINT ( 'NONE',  ( -0.6527133886630747117, 8.860760056385830197, -7.903039949738215775 ) ) ;
#4616 = ORIENTED_EDGE ( 'NONE', *, *, #4388, .F. ) ;
#4617 = ORIENTED_EDGE ( 'NONE', *, *, #69, .F. ) ;
#4618 = EDGE_CURVE ( 'NONE', #79, #6584, #8194, .T. ) ;
#4619 = CARTESIAN_POINT ( 'NONE',  ( -7.999999999999888978, -3.098204225878262719, -8.084209322808188602 ) ) ;
#4620 = ORIENTED_EDGE ( 'NONE', *, *, #1968, .F. ) ;
#4621 = CARTESIAN_POINT ( 'NONE',  ( 0.000000000000000000, 0.000000000000000000, 0.000000000000000000 ) ) ;
#4622 = CARTESIAN_POINT ( 'NONE',  ( 8.000000000000007105, 4.618802153516899267, -0.7145311798163467287 ) ) ;
#4623 =( REPRESENTATION_RELATIONSHIP ('NONE','NONE', #1279, #6969 ) REPRESENTATION_RELATIONSHIP_WITH_TRANSFORMATION ( #6756 )SHAPE_REPRESENTATION_RELATIONSHIP( ) );
#4624 = FACE_BOUND ( 'NONE', #8145, .T. ) ;
#4625 = ORIENTED_EDGE ( 'NONE', *, *, #5607, .F. ) ;
#4626 = CARTESIAN_POINT ( 'NONE',  ( 0.000000000000000000, 0.000000000000000000, -8.400000000000018119 ) ) ;
#4627 = ADVANCED_FACE ( 'NONE', ( #7416 ), #6815, .F. ) ;
#4628 = AXIS2_PLACEMENT_3D ( 'NONE', #4905, #5624, #3605 ) ;
#4629 = EDGE_CURVE ( 'NONE', #477, #4794, #6775, .T. ) ;
#4630 = DIRECTION ( 'NONE',  ( -3.851859888774471706E-33, -1.232595164407830946E-32, -1.000000000000000000 ) ) ;
#4631 = AXIS2_PLACEMENT_3D ( 'NONE', #5954, #1924, #4583 ) ;
#4632 = DIRECTION ( 'NONE',  ( 6.400024471206997542E-36, -1.000000000000000000, -7.598173571352216173E-18 ) ) ;
#4633 = AXIS2_PLACEMENT_3D ( 'NONE', #5792, #5228, #4976 ) ;
#4634 = FACE_OUTER_BOUND ( 'NONE', #8001, .T. ) ;
#4635 = ORIENTED_EDGE ( 'NONE', *, *, #3763, .F. ) ;
#4636 = APPLICATION_CONTEXT ( 'automotive_design' ) ;
#4637 = CARTESIAN_POINT ( 'NONE',  ( 5.510910596163084034E-15, 39.99999999999992184, -120.0000000000000000 ) ) ;
#4638 = B_SPLINE_CURVE_WITH_KNOTS ( 'NONE', 3,
 ( #5979, #734, #2041, #2090, #3344, #1343, #4615, #5263 ),
 .UNSPECIFIED., .F., .F.,
 ( 4, 2, 2, 4 ),
 ( 0.004673709593152869553, 0.005837709341828217595, 0.007001709090503566504, 0.009329708587854264323 ),
 .UNSPECIFIED. ) ;
#4639 = AXIS2_PLACEMENT_3D ( 'NONE', #4506, #586, #4600 ) ;
#4640 = DIRECTION ( 'NONE',  ( 0.000000000000000000, 0.000000000000000000, -1.000000000000000000 ) ) ;
#4641 = ORIENTED_EDGE ( 'NONE', *, *, #8323, .F. ) ;
#4642 = EDGE_CURVE ( 'NONE', #8489, #367, #7283, .T. ) ;
#4643 = CIRCLE ( 'NONE', #2544, 5.500000000000023981 ) ;
#4644 = FACE_OUTER_BOUND ( 'NONE', #3450, .T. ) ;
#4645 = EDGE_LOOP ( 'NONE', ( #3537, #5892, #6391, #3820 ) ) ;
#4646 = AXIS2_PLACEMENT_3D ( 'NONE', #7751, #6985, #5648 ) ;
#4647 = DIRECTION ( 'NONE',  ( -0.000000000000000000, -0.000000000000000000, 1.000000000000000000 ) ) ;
#4648 = VECTOR ( 'NONE', #2184, 1000.000000000000114 ) ;
#4649 = LINE ( 'NONE', #6692, #8503 ) ;
#4650 = DIRECTION ( 'NONE',  ( -1.000000000000000000, -8.881784197001244435E-16, 0.000000000000000000 ) ) ;
#4651 = AXIS2_PLACEMENT_3D ( 'NONE', #3501, #4769, #976 ) ;
#4652 = CARTESIAN_POINT ( 'NONE',  ( -54.49999999999963052, 87.50000000000034106, 9.999999999999786837 ) ) ;
#4653 = EDGE_LOOP ( 'NONE', ( #2116, #4978, #7483, #6367 ) ) ;
#4654 = CARTESIAN_POINT ( 'NONE',  ( 5.000000000000115463, 2.342598717236854977, -4.057500000000047180 ) ) ;
#4655 = VERTEX_POINT ( 'NONE', #3496 ) ;
#4656 = CARTESIAN_POINT ( 'NONE',  ( -5.080504117408896292, -2.106769544347821377, -8.400999999999992696 ) ) ;
#4657 = UNCERTAINTY_MEASURE_WITH_UNIT (LENGTH_MEASURE( 1.000000000000000082E-05 ), #5392, 'distance_accuracy_value', 'NONE');
#4658 = DIRECTION ( 'NONE',  ( -1.000000000000000000, 2.842664852890546338E-35, 1.540743955509788340E-33 ) ) ;
#4659 = DIRECTION ( 'NONE',  ( 1.000000000000000000, 3.083952846180992055E-15, -5.478200730701473829E-30 ) ) ;
#4660 = CARTESIAN_POINT ( 'NONE',  ( 0.6527133886632227044, -8.860760056385986516, -7.903039949738120740 ) ) ;
#4661 = CARTESIAN_POINT ( 'NONE',  ( 5.000000000000004441, -2.342598717236951789, 4.057500000000047180 ) ) ;
#4662 = ORIENTED_EDGE ( 'NONE', *, *, #2474, .T. ) ;
#4663 = EDGE_CURVE ( 'NONE', #6630, #1742, #330, .T. ) ;
#4664 = ORIENTED_EDGE ( 'NONE', *, *, #3734, .F. ) ;
#4665 = AXIS2_PLACEMENT_3D ( 'NONE', #7449, #6800, #5492 ) ;
#4666 = PLANE ( 'NONE',  #2261 ) ;
#4667 = ORIENTED_EDGE ( 'NONE', *, *, #1190, .T. ) ;
#4668 = DIRECTION ( 'NONE',  ( 3.851859888774471706E-33, 1.232595164407830946E-32, 1.000000000000000000 ) ) ;
#4669 = AXIS2_PLACEMENT_3D ( 'NONE', #7144, #4402, #7062 ) ;
#4670 = FACE_OUTER_BOUND ( 'NONE', #1725, .T. ) ;
#4671 = CARTESIAN_POINT ( 'NONE',  ( -8.000000000000000000, -3.098204225878149920, -8.084209322808149523 ) ) ;
#4672 = CARTESIAN_POINT ( 'NONE',  ( 4.000000000000003553, 1.759474945355415931, -3.047500000000091802 ) ) ;
#4673 = PRODUCT_DEFINITION ( 'UNKNOWN', '', #3259, #4208 ) ;
#4674 = ORIENTED_EDGE ( 'NONE', *, *, #7834, .F. ) ;
#4675 = FACE_OUTER_BOUND ( 'NONE', #7828, .T. ) ;
#4676 = ORIENTED_EDGE ( 'NONE', *, *, #1603, .F. ) ;
#4677 = ITEM_DEFINED_TRANSFORMATION ( 'NONE', 'NONE', #6596,  #7563 ) ;
#4678 = DIRECTION ( 'NONE',  ( -1.000000000000000000, 0.000000000000000000, 0.000000000000000000 ) ) ;
#4679 = AXIS2_PLACEMENT_3D ( 'NONE', #1995, #7261, #4659 ) ;
#4680 = ADVANCED_FACE ( 'NONE', ( #2843 ), #885, .T. ) ;
#4681 = ORIENTED_EDGE ( 'NONE', *, *, #6764, .F. ) ;
#4682 = DIRECTION ( 'NONE',  ( 0.000000000000000000, -5.322451846059955323E-30, 1.000000000000000000 ) ) ;
#4683 = AXIS2_PLACEMENT_3D ( 'NONE', #7691, #7083, #1115 ) ;
#4684 = ORIENTED_EDGE ( 'NONE', *, *, #1962, .F. ) ;
#4685 = FACE_BOUND ( 'NONE', #3124, .T. ) ;
#4686 = ORIENTED_EDGE ( 'NONE', *, *, #5995, .T. ) ;
#4687 = CARTESIAN_POINT ( 'NONE',  ( 5.551115123125782702E-14, 3.518949890710790118, 2.220446049250313081E-13 ) ) ;
#4688 = AXIS2_PLACEMENT_3D ( 'NONE', #7250, #2025, #4689 ) ;
#4689 = DIRECTION ( 'NONE',  ( 0.9237280213470678847, 0.3830490080632384942, 0.000000000000000000 ) ) ;
#4690 = ADVANCED_FACE ( 'NONE', ( #1133, #3754 ), #6414, .T. ) ;
#4691 = DIRECTION ( 'NONE',  ( 0.000000000000000000, 0.000000000000000000, -1.000000000000000000 ) ) ;
#4692 = CARTESIAN_POINT ( 'NONE',  ( 0.000000000000000000, 0.000000000000000000, -8.400000000000018119 ) ) ;
#4693 = DIRECTION ( 'NONE',  ( -1.000000000000000000, -8.881784197001244435E-16, 0.000000000000000000 ) ) ;
#4694 = ORIENTED_EDGE ( 'NONE', *, *, #535, .T. ) ;
#4695 = DIRECTION ( 'NONE',  ( -1.000000000000000000, -8.881784197001244435E-16, 0.000000000000000000 ) ) ;
#4696 = VERTEX_POINT ( 'NONE', #6938 ) ;
#4697 = DIRECTION ( 'NONE',  ( 0.9237280213470678847, 0.3830490080632384942, 0.000000000000000000 ) ) ;
#4698 = AXIS2_PLACEMENT_3D ( 'NONE', #4610, #7259, #6655 ) ;
#4699 = LINE ( 'NONE', #7345, #8301 ) ;
#4700 = CARTESIAN_POINT ( 'NONE',  ( -4.680456609904073417, -6.535341423375602865, -8.383111142572214902 ) ) ;
#4701 = DIRECTION ( 'NONE',  ( -1.000000000000000000, 1.774937036747276562E-30, 0.000000000000000000 ) ) ;
#4702 = ADVANCED_FACE ( 'NONE', ( #967 ), #2394, .F. ) ;
#4703 = CARTESIAN_POINT ( 'NONE',  ( -19.99999999999982947, 15.00000000000012434, 10.00000000000000888 ) ) ;
#4704 = CARTESIAN_POINT ( 'NONE',  ( -8.000000000000225597, 0.7809653281575846817, -8.399999999999884892 ) ) ;
#4705 = EDGE_LOOP ( 'NONE', ( #8238, #4664, #3055, #8474 ) ) ;
#4706 = CARTESIAN_POINT ( 'NONE',  ( -8.000000000000117240, -1.110223024625156540E-13, 0.000000000000000000 ) ) ;
#4707 = VERTEX_POINT ( 'NONE', #307 ) ;
#4708 = CARTESIAN_POINT ( 'NONE',  ( 8.000000000000341061, 6.499999999999922728, 8.881784197001252323E-13 ) ) ;
#4709 = DIRECTION ( 'NONE',  ( 0.000000000000000000, -0.4999999999999989453, 0.8660254037844392627 ) ) ;
#4710 = EDGE_CURVE ( 'NONE', #749, #7867, #473, .T. ) ;
#4711 = FACE_OUTER_BOUND ( 'NONE', #1010, .T. ) ;
#4712 = PLANE ( 'NONE',  #7975 ) ;
#4713 = CARTESIAN_POINT ( 'NONE',  ( 0.000000000000000000, 0.000000000000000000, -109.9999999999999574 ) ) ;
#4714 = ORIENTED_EDGE ( 'NONE', *, *, #7195, .T. ) ;
#4715 = ORIENTED_EDGE ( 'NONE', *, *, #3346, .T. ) ;
#4716 = VECTOR ( 'NONE', #6999, 1000.000000000000000 ) ;
#4717 = EDGE_CURVE ( 'NONE', #1200, #3424, #3090, .T. ) ;
#4718 = CARTESIAN_POINT ( 'NONE',  ( 8.000000000000015987, -3.867591403079595480, -7.902324684675320121 ) ) ;
#4719 = EDGE_LOOP ( 'NONE', ( #1421, #8540, #2055 ) ) ;
#4720 = VECTOR ( 'NONE', #5943, 1000.000000000000000 ) ;
#4721 = CARTESIAN_POINT ( 'NONE',  ( 0.6543471694414042528, 8.859816792613671055, -0.4964154566688170900 ) ) ;
#4722 = VECTOR ( 'NONE', #2179, 1000.000000000000000 ) ;
#4723 = CIRCLE ( 'NONE', #542, 5.499999999999999112 ) ;
#4724 = ORIENTED_EDGE ( 'NONE', *, *, #2678, .F. ) ;
#4725 = FACE_OUTER_BOUND ( 'NONE', #7797, .T. ) ;
#4726 = VERTEX_POINT ( 'NONE', #5781 ) ;
#4727 = DIRECTION ( 'NONE',  ( -1.000000000000000000, -8.881784197001244435E-16, -0.000000000000000000 ) ) ;
#4728 = ADVANCED_FACE ( 'NONE', ( #8412 ), #2438, .F. ) ;
#4729 = AXIS2_PLACEMENT_3D ( 'NONE', #3987, #680, #192 ) ;
#4730 = CONICAL_SURFACE ( 'NONE', #1101, 70.00000000000008527, 0.7853981633974441712 ) ;
#4731 = CARTESIAN_POINT ( 'NONE',  ( 0.000000000000000000, 0.000000000000000000, -50.00000000000000000 ) ) ;
#4732 = CIRCLE ( 'NONE', #3624, 8.000000000000000000 ) ;
#4733 = CARTESIAN_POINT ( 'NONE',  ( 8.000000000000008882, 3.115336682266736101, -8.080606868608565918 ) ) ;
#4734 = CARTESIAN_POINT ( 'NONE',  ( 8.000000000000120792, -0.7805016046292556631, -7.994805175954437918E-14 ) ) ;
#4735 =( NAMED_UNIT ( * ) PLANE_ANGLE_UNIT ( ) SI_UNIT ( $, .RADIAN. ) );
#4736 = ORIENTED_EDGE ( 'NONE', *, *, #5380, .F. ) ;
#4737 = AXIS2_PLACEMENT_3D ( 'NONE', #6368, #8232, #7053 ) ;
#4738 = FACE_BOUND ( 'NONE', #6008, .T. ) ;
#4739 = SURFACE_STYLE_USAGE ( .BOTH. , #5442 ) ;
#4740 = DIRECTION ( 'NONE',  ( -1.000000000000000000, 1.774937036747276562E-30, 0.000000000000000000 ) ) ;
#4741 = ADVANCED_FACE ( 'NONE', ( #1645 ), #4321, .F. ) ;
#4742 = UNCERTAINTY_MEASURE_WITH_UNIT (LENGTH_MEASURE( 1.000000000000000082E-05 ), #5304, 'distance_accuracy_value', 'NONE');
#4743 = CARTESIAN_POINT ( 'NONE',  ( -3.318518101603116666, -7.321656987762883873, -2.620211719036452669E-14 ) ) ;
#4744 = AXIS2_PLACEMENT_3D ( 'NONE', #5441, #2133, #8601 ) ;
#4745 = PRODUCT_DEFINITION_SHAPE ( 'NONE', 'NONE',  #8614 ) ;
#4746 = CARTESIAN_POINT ( 'NONE',  ( 6.686525924292292977, -5.377136764700166438, -8.083279549040401690 ) ) ;
#4747 = CARTESIAN_POINT ( 'NONE',  ( -31.74999999999994316, 0.000000000000000000, 0.000000000000000000 ) ) ;
#4748 = ITEM_DEFINED_TRANSFORMATION ( 'NONE', 'NONE', #7577,  #7563 ) ;
#4749 = FACE_OUTER_BOUND ( 'NONE', #6200, .T. ) ;
#4750 = DIRECTION ( 'NONE',  ( -7.703719777548943412E-34, 0.000000000000000000, 1.000000000000000000 ) ) ;
#4751 = ORIENTED_EDGE ( 'NONE', *, *, #5373, .T. ) ;
#4752 = CARTESIAN_POINT ( 'NONE',  ( 0.000000000000000000, -3.469446951953614189E-15, 130.0000000000000000 ) ) ;
#4753 = ORIENTED_EDGE ( 'NONE', *, *, #2038, .F. ) ;
#4754 = EDGE_CURVE ( 'NONE', #2122, #4141, #4364, .T. ) ;
#4755 = DIRECTION ( 'NONE',  ( 0.000000000000000000, 5.322451846059955323E-30, -1.000000000000000000 ) ) ;
#4756 = VERTEX_POINT ( 'NONE', #3870 ) ;
#4757 = DIRECTION ( 'NONE',  ( 0.000000000000000000, 0.000000000000000000, 1.000000000000000000 ) ) ;
#4758 = EDGE_LOOP ( 'NONE', ( #1211, #2230, #839, #5512, #4792, #3418 ) ) ;
#4759 = DIRECTION ( 'NONE',  ( -1.774937036747276212E-30, 0.5000000000000009992, 0.8660254037844380415 ) ) ;
#4760 = EDGE_LOOP ( 'NONE', ( #2476, #3642, #7942, #7315 ) ) ;
#4761 = EDGE_LOOP ( 'NONE', ( #3468, #7355, #7412 ) ) ;
#4762 = ADVANCED_FACE ( 'NONE', ( #4482, #6628 ), #3914, .F. ) ;
#4763 = EDGE_CURVE ( 'NONE', #6543, #6339, #5819, .T. ) ;
#4764 = DIRECTION ( 'NONE',  ( 1.774937036747276212E-30, -0.5000000000000009992, -0.8660254037844380415 ) ) ;
#4765 = AXIS2_PLACEMENT_3D ( 'NONE', #6743, #5600, #2347 ) ;
#4766 = ORIENTED_EDGE ( 'NONE', *, *, #5764, .T. ) ;
#4767 = DIRECTION ( 'NONE',  ( -3.851859888774471706E-33, -1.232595164407830946E-32, -1.000000000000000000 ) ) ;
#4768 = CARTESIAN_POINT ( 'NONE',  ( -7.999999999999785061, 4.618802153516870845, -7.685468820183672278 ) ) ;
#4769 = DIRECTION ( 'NONE',  ( 0.000000000000000000, 0.000000000000000000, 1.000000000000000000 ) ) ;
#4770 = ORIENTED_EDGE ( 'NONE', *, *, #1434, .F. ) ;
#4771 = DIRECTION ( 'NONE',  ( -1.000000000000000000, -8.881784197001244435E-16, 0.000000000000000000 ) ) ;
#4772 = ORIENTED_EDGE ( 'NONE', *, *, #796, .F. ) ;
#4773 = DIRECTION ( 'NONE',  ( -1.000000000000000000, 0.000000000000000000, 0.000000000000000000 ) ) ;
#4774 = DIRECTION ( 'NONE',  ( -1.000000000000000000, -8.881784197001244435E-16, 0.000000000000000000 ) ) ;
#4775 = VERTEX_POINT ( 'NONE', #1354 ) ;
#4776 = DIRECTION ( 'NONE',  ( -0.5000000000000044409, 1.060575238725013534E-16, -0.8660254037844360431 ) ) ;
#4777 = CIRCLE ( 'NONE', #7135, 25.00000000000000711 ) ;
#4778 = AXIS2_PLACEMENT_3D ( 'NONE', #7107, #5182, #5662 ) ;
#4779 = DIRECTION ( 'NONE',  ( -3.851859888774471706E-33, -1.232595164407830946E-32, -1.000000000000000000 ) ) ;
#4780 = EDGE_CURVE ( 'NONE', #7888, #3413, #564, .T. ) ;
#4781 = PLANE ( 'NONE',  #5088 ) ;
#4782 = CYLINDRICAL_SURFACE ( 'NONE', #7981, 25.00000000000000711 ) ;
#4783 = ORIENTED_EDGE ( 'NONE', *, *, #4618, .F. ) ;
#4784 = CARTESIAN_POINT ( 'NONE',  ( 0.000000000000000000, 0.000000000000000000, 0.000000000000000000 ) ) ;
#4785 = CARTESIAN_POINT ( 'NONE',  ( -275.0000000000000000, -425.0000000000000000, -80.00000000000000000 ) ) ;
#4786 = CARTESIAN_POINT ( 'NONE',  ( -6.689127551062022725, -5.375634714784609081, -0.3173508448886571132 ) ) ;
#4787 = AXIS2_PLACEMENT_3D ( 'NONE', #6634, #3411, #6724 ) ;
#4788 = CARTESIAN_POINT ( 'NONE',  ( 10.00000000000012079, -29.14213562373080180, -20.00000000000001776 ) ) ;
#4789 = FACE_OUTER_BOUND ( 'NONE', #4332, .T. ) ;
#4790 = ADVANCED_FACE ( 'NONE', ( #4670 ), #5951, .F. ) ;
#4791 = CARTESIAN_POINT ( 'NONE',  ( -5.354491962338311595, 6.146186931204400850, -8.331901280394522047 ) ) ;
#4792 = ORIENTED_EDGE ( 'NONE', *, *, #3549, .F. ) ;
#4793 = CARTESIAN_POINT ( 'NONE',  ( -8.000000000000664357, -1.555946510855795273, -0.06708870216369239303 ) ) ;
#4794 = VERTEX_POINT ( 'NONE', #7318 ) ;
#4795 = CARTESIAN_POINT ( 'NONE',  ( 7.347286611336957485, 4.995646404165020371, -7.903039949738357883 ) ) ;
#4796 = LINE ( 'NONE', #5455, #6050 ) ;
#4797 = LINE ( 'NONE', #6078, #2052 ) ;
#4798 = ORIENTED_EDGE ( 'NONE', *, *, #3019, .F. ) ;
#4799 = CARTESIAN_POINT ( 'NONE',  ( 2.644994884459147766, -7.710515798486462735, -0.08224679563977427277 ) ) ;
#4800 = ORIENTED_EDGE ( 'NONE', *, *, #7084, .F. ) ;
#4801 = AXIS2_PLACEMENT_3D ( 'NONE', #5141, #4492, #5874 ) ;
#4802 = ADVANCED_FACE ( 'NONE', ( #8573, #2574, #3222, #1312, #4006, #1963 ), #2526, .T. ) ;
#4803 = CARTESIAN_POINT ( 'NONE',  ( 0.000000000000000000, 0.000000000000000000, -8.400000000000018119 ) ) ;
#4804 = VERTEX_POINT ( 'NONE', #3968 ) ;
#4805 = VECTOR ( 'NONE', #8056, 1000.000000000000000 ) ;
#4806 = PRODUCT_DEFINITION_SHAPE ( 'NONE', 'NONE',  #8624 ) ;
#4807 = FACE_OUTER_BOUND ( 'NONE', #2839, .T. ) ;
#4808 = EDGE_CURVE ( 'NONE', #579, #4536, #3293, .T. ) ;
#4809 = ORIENTED_EDGE ( 'NONE', *, *, #5156, .F. ) ;
#4810 = ADVANCED_FACE ( 'NONE', ( #3830 ), #7794, .F. ) ;
#4811 = DIRECTION ( 'NONE',  ( -7.703719777548943412E-34, 0.000000000000000000, 1.000000000000000000 ) ) ;
#4812 = DIRECTION ( 'NONE',  ( 0.000000000000000000, 0.000000000000000000, -1.000000000000000000 ) ) ;
#4813 = CARTESIAN_POINT ( 'NONE',  ( -350.0000000000001137, 0.000000000000000000, -49.99999999999998579 ) ) ;
#4814 = ORIENTED_EDGE ( 'NONE', *, *, #4224, .T. ) ;
#4815 = ORIENTED_EDGE ( 'NONE', *, *, #1608, .F. ) ;
#4816 = DIRECTION ( 'NONE',  ( 0.000000000000000000, 0.000000000000000000, -1.000000000000000000 ) ) ;
#4817 = CARTESIAN_POINT ( 'NONE',  ( 0.000000000000000000, 32.50000000000005684, -6.938893903907228378E-15 ) ) ;
#4818 = ORIENTED_EDGE ( 'NONE', *, *, #5652, .T. ) ;
#4819 = LINE ( 'NONE', #8088, #6275 ) ;
#4820 = CARTESIAN_POINT ( 'NONE',  ( 7.999999999999674039, -4.618802153517231446, -7.685468820183672278 ) ) ;
#4821 = EDGE_LOOP ( 'NONE', ( #4620, #6513, #4517, #5324 ) ) ;
#4822 = FACE_BOUND ( 'NONE', #6103, .T. ) ;
#4823 =( LENGTH_UNIT ( ) NAMED_UNIT ( * ) SI_UNIT ( .MILLI., .METRE. ) );
#4824 = DIRECTION ( 'NONE',  ( -1.000000000000000000, 0.000000000000000000, 0.000000000000000000 ) ) ;
#4825 = DIRECTION ( 'NONE',  ( 0.000000000000000000, -0.4999999999999983902, 0.8660254037844395958 ) ) ;
#4826 = FILL_AREA_STYLE_COLOUR ( '', #2360 ) ;
#4827 = CARTESIAN_POINT ( 'NONE',  ( 8.400000000000018119, -5.551115123125782702E-14, 6.661338147750939243E-13 ) ) ;
#4828 = CARTESIAN_POINT ( 'NONE',  ( 275.0000000000000000, -425.0000000000000000, 80.00000000000000000 ) ) ;
#4829 = VERTEX_POINT ( 'NONE', #5065 ) ;
#4830 = AXIS2_PLACEMENT_3D ( 'NONE', #489, #5129, #3265 ) ;
#4831 = VERTEX_POINT ( 'NONE', #8492 ) ;
#4832 = DIRECTION ( 'NONE',  ( 1.000000000000000000, -1.774937036747276562E-30, 0.000000000000000000 ) ) ;
#4833 = EDGE_CURVE ( 'NONE', #4401, #2122, #7045, .T. ) ;
#4834 = CARTESIAN_POINT ( 'NONE',  ( 4.000000000000003553, 9.714451465470115942E-14, 3.047499999999999876 ) ) ;
#4835 = ORIENTED_EDGE ( 'NONE', *, *, #48, .F. ) ;
#4836 = LINE ( 'NONE', #961, #3457 ) ;
#4837 = VERTEX_POINT ( 'NONE', #5181 ) ;
#4838 = DIRECTION ( 'NONE',  ( -0.000000000000000000, -0.000000000000000000, 1.000000000000000000 ) ) ;
#4839 = EDGE_LOOP ( 'NONE', ( #1591, #1176, #7706, #4814 ) ) ;
#4840 = EDGE_CURVE ( 'NONE', #7606, #2641, #7837, .T. ) ;
#4841 = DIRECTION ( 'NONE',  ( 0.000000000000000000, -1.064348848528640545E-29, 1.000000000000000000 ) ) ;
#4842 = B_SPLINE_CURVE_WITH_KNOTS ( 'NONE', 3,
 ( #2836, #3354, #4671, #6629, #2752, #5992 ),
 .UNSPECIFIED., .F., .F.,
 ( 4, 2, 4 ),
 ( 0.008240550023493522364, 0.01057684187039419771, 0.01291313371729487305 ),
 .UNSPECIFIED. ) ;
#4843 = ORIENTED_EDGE ( 'NONE', *, *, #7810, .T. ) ;
#4844 = DIRECTION ( 'NONE',  ( 0.000000000000000000, -1.213383262747659708E-29, 1.000000000000000000 ) ) ;
#4845 = DIRECTION ( 'NONE',  ( 0.9237280213470682178, 0.3830490080632377725, 0.000000000000000000 ) ) ;
#4846 = VERTEX_POINT ( 'NONE', #7925 ) ;
#4847 = AXIS2_PLACEMENT_3D ( 'NONE', #2825, #8178, #7656 ) ;
#4848 = DIRECTION ( 'NONE',  ( 0.000000000000000000, 5.322451846059954622E-30, -1.000000000000000000 ) ) ;
#4849 = EDGE_LOOP ( 'NONE', ( #879, #6759 ) ) ;
#4850 = DIRECTION ( 'NONE',  ( 0.000000000000000000, 0.000000000000000000, -1.000000000000000000 ) ) ;
#4851 = ADVANCED_FACE ( 'NONE', ( #4531 ), #7190, .F. ) ;
#4852 = VECTOR ( 'NONE', #7349, 1000.000000000000000 ) ;
#4853 = FACE_OUTER_BOUND ( 'NONE', #1731, .T. ) ;
#4854 = ORIENTED_EDGE ( 'NONE', *, *, #7775, .T. ) ;
#4855 = DIRECTION ( 'NONE',  ( -3.549874073494553124E-30, -1.000000000000000000, -1.064348848528640545E-29 ) ) ;
#4856 = ORIENTED_EDGE ( 'NONE', *, *, #6794, .T. ) ;
#4857 = EDGE_CURVE ( 'NONE', #4033, #7559, #401, .T. ) ;
#4858 =( REPRESENTATION_RELATIONSHIP ('NONE','NONE', #1279, #5506 ) REPRESENTATION_RELATIONSHIP_WITH_TRANSFORMATION ( #1318 )SHAPE_REPRESENTATION_RELATIONSHIP( ) );
#4859 = FACE_OUTER_BOUND ( 'NONE', #2434, .T. ) ;
#4860 = ORIENTED_EDGE ( 'NONE', *, *, #1562, .F. ) ;
#4861 = AXIS2_PLACEMENT_3D ( 'NONE', #7374, #7988, #7549 ) ;
#4862 = AXIS2_PLACEMENT_3D ( 'NONE', #1580, #8293, #6905 ) ;
#4863 = CARTESIAN_POINT ( 'NONE',  ( 50.00000000000004263, -500.0000000000000000, 50.00000000000000000 ) ) ;
#4864 = AXIS2_PLACEMENT_3D ( 'NONE', #1104, #1752, #3727 ) ;
#4865 = DIRECTION ( 'NONE',  ( 0.000000000000000000, 0.000000000000000000, -1.000000000000000000 ) ) ;
#4866 = DIRECTION ( 'NONE',  ( -0.000000000000000000, -0.000000000000000000, 1.000000000000000000 ) ) ;
#4867 = B_SPLINE_CURVE_WITH_KNOTS ( 'NONE', 3,
 ( #613, #6115, #3263, #74, #5948, #6030 ),
 .UNSPECIFIED., .F., .F.,
 ( 4, 2, 4 ),
 ( 2.380731626810675838E-07, 0.002336973833157153513, 0.004673709593151625756 ),
 .UNSPECIFIED. ) ;
#4868 =( NAMED_UNIT ( * ) SI_UNIT ( $, .STERADIAN. ) SOLID_ANGLE_UNIT ( ) );
#4869 = CIRCLE ( 'NONE', #984, 4.171999999999999709 ) ;
#4870 = DIRECTION ( 'NONE',  ( -0.000000000000000000, -0.000000000000000000, 1.000000000000000000 ) ) ;
#4871 = VECTOR ( 'NONE', #2322, 1000.000000000000000 ) ;
#4872 = DIRECTION ( 'NONE',  ( -3.851859888774471706E-33, -1.232595164407830946E-32, -1.000000000000000000 ) ) ;
#4873 = ORIENTED_EDGE ( 'NONE', *, *, #5772, .F. ) ;
#4874 = CLOSED_SHELL ( 'NONE', ( #2587, #1276, #3049, #1860, #4255, #5728, #474, #6602, #6656, #372, #2496, #3484, #1029, #5317, #6785, #665, #8378, #4741, #1014, #3539, #8424, #4802, #5674, #2879, #1362, #6802, #2273, #6033, #8519, #6254, #1057, #4304, #8084 ) ) ;
#4875 = DIRECTION ( 'NONE',  ( 1.000000000000000000, -1.774937036747276562E-30, -9.447016907875728896E-60 ) ) ;
#4876 = ORIENTED_EDGE ( 'NONE', *, *, #7217, .F. ) ;
#4877 = CARTESIAN_POINT ( 'NONE',  ( -8.000000000000001776, 0.7809653281576651729, -8.332263102140549280E-15 ) ) ;
#4878 = CIRCLE ( 'NONE', #1961, 19.49999999999996803 ) ;
#4879 = CARTESIAN_POINT ( 'NONE',  ( -32.49999999999997158, 3.469446951953614189E-15, 18.00000000000000355 ) ) ;
#4880 = ORIENTED_EDGE ( 'NONE', *, *, #3840, .F. ) ;
#4881 = CARTESIAN_POINT ( 'NONE',  ( -8.000000000000673239, 4.618802153517287401, -7.685468820183672278 ) ) ;
#4882 = ORIENTED_EDGE ( 'NONE', *, *, #5147, .T. ) ;
#4883 = VERTEX_POINT ( 'NONE', #167 ) ;
#4884 = EDGE_CURVE ( 'NONE', #282, #2762, #4797, .T. ) ;
#4885 = DIRECTION ( 'NONE',  ( 1.000000000000000000, -0.000000000000000000, -6.938893903907228378E-17 ) ) ;
#4886 = ORIENTED_EDGE ( 'NONE', *, *, #7969, .F. ) ;
#4887 = CARTESIAN_POINT ( 'NONE',  ( 6.720025694767354167E-35, -10.50000000000001421, 130.0000000000000000 ) ) ;
#4888 = EDGE_CURVE ( 'NONE', #2971, #3548, #4948, .T. ) ;
#4889 = DIRECTION ( 'NONE',  ( 0.000000000000000000, -1.000000000000000000, -1.795949010423047620E-16 ) ) ;
#4890 = DIRECTION ( 'NONE',  ( -4.579669976578766785E-16, -5.898059818321121934E-17, -1.000000000000000000 ) ) ;
#4891 = ORIENTED_EDGE ( 'NONE', *, *, #5549, .F. ) ;
#4892 = CARTESIAN_POINT ( 'NONE',  ( 20.00000000000011724, -14.99999999999990230, -20.00000000000001776 ) ) ;
#4893 = ORIENTED_EDGE ( 'NONE', *, *, #7500, .F. ) ;
#4894 = DIRECTION ( 'NONE',  ( 2.960372000631175920E-34, -1.000000000000000000, -4.592425496802573602E-17 ) ) ;
#4895 = CYLINDRICAL_SURFACE ( 'NONE', #6581, 5.500000000000024869 ) ;
#4896 = DIRECTION ( 'NONE',  ( 1.000000000000000000, 0.000000000000000000, 0.000000000000000000 ) ) ;
#4897 = EDGE_LOOP ( 'NONE', ( #3866, #3399, #3982 ) ) ;
#4898 = AXIS2_PLACEMENT_3D ( 'NONE', #32, #6321, #2211 ) ;
#4899 = DIRECTION ( 'NONE',  ( 6.400024471207000214E-36, -1.000000000000000000, 0.000000000000000000 ) ) ;
#4900 = PLANE ( 'NONE',  #3009 ) ;
#4901 = EDGE_CURVE ( 'NONE', #4915, #3572, #2149, .T. ) ;
#4902 = ORIENTED_EDGE ( 'NONE', *, *, #3361, .F. ) ;
#4903 = AXIS2_PLACEMENT_3D ( 'NONE', #5670, #1669, #7607 ) ;
#4904 = ORIENTED_EDGE ( 'NONE', *, *, #4629, .F. ) ;
#4905 = CARTESIAN_POINT ( 'NONE',  ( -49.99999999999954525, 120.0000000000003268, 0.000000000000000000 ) ) ;
#4906 = DIRECTION ( 'NONE',  ( 1.000000000000000000, 8.881784197001244435E-16, 0.000000000000000000 ) ) ;
#4907 = AXIS2_PLACEMENT_3D ( 'NONE', #5069, #1187, #4503 ) ;
#4908 = EDGE_CURVE ( 'NONE', #2054, #3833, #3722, .T. ) ;
#4909 = DIRECTION ( 'NONE',  ( 1.000000000000000000, -0.000000000000000000, -6.938893903907228378E-17 ) ) ;
#4910 = ADVANCED_FACE ( 'NONE', ( #998 ), #5407, .T. ) ;
#4911 = CARTESIAN_POINT ( 'NONE',  ( -9.587279263159650267E-30, 410.0000000000000000, 24.49999999999993605 ) ) ;
#4912 = CARTESIAN_POINT ( 'NONE',  ( 8.000000000000015987, -3.098204225878660623, -0.3157906771919842814 ) ) ;
#4913 = ORIENTED_EDGE ( 'NONE', *, *, #3984, .F. ) ;
#4914 = DIRECTION ( 'NONE',  ( 0.5000000000000029976, -0.8660254037844370423, 0.000000000000000000 ) ) ;
#4915 = VERTEX_POINT ( 'NONE', #5499 ) ;
#4916 = CIRCLE ( 'NONE', #1026, 5.749999999999991118 ) ;
#4917 = AXIS2_PLACEMENT_3D ( 'NONE', #3007, #6335, #358 ) ;
#4918 =( GEOMETRIC_REPRESENTATION_CONTEXT ( 3 ) GLOBAL_UNCERTAINTY_ASSIGNED_CONTEXT ( ( #1132 ) ) GLOBAL_UNIT_ASSIGNED_CONTEXT ( ( #1546, #860, #7644 ) ) REPRESENTATION_CONTEXT ( 'NONE', 'WORKASPACE' ) );
#4919 = EDGE_CURVE ( 'NONE', #3370, #4252, #1903, .T. ) ;
#4920 = PLANE ( 'NONE',  #1576 ) ;
#4921 = DIRECTION ( 'NONE',  ( 0.000000000000000000, 0.000000000000000000, 1.000000000000000000 ) ) ;
#4922 = ORIENTED_EDGE ( 'NONE', *, *, #8048, .T. ) ;
#4923 = ORIENTED_EDGE ( 'NONE', *, *, #2339, .F. ) ;
#4924 =( GEOMETRIC_REPRESENTATION_CONTEXT ( 3 ) GLOBAL_UNCERTAINTY_ASSIGNED_CONTEXT ( ( #5050 ) ) GLOBAL_UNIT_ASSIGNED_CONTEXT ( ( #3688, #376, #3067 ) ) REPRESENTATION_CONTEXT ( 'NONE', 'WORKASPACE' ) );
#4925 = ADVANCED_FACE ( 'NONE', ( #4711 ), #2103, .F. ) ;
#4926 = PRODUCT_DEFINITION ( 'UNKNOWN', '', #3542, #8548 ) ;
#4927 = VECTOR ( 'NONE', #4750, 1000.000000000000000 ) ;
#4928 = CARTESIAN_POINT ( 'NONE',  ( -6.661338147750939243E-13, 9.237604307034352757, -0.7145311798163467287 ) ) ;
#4929 = CARTESIAN_POINT ( 'NONE',  ( 0.000000000000000000, 0.000000000000000000, 45.00000000000000000 ) ) ;
#4930 = ORIENTED_EDGE ( 'NONE', *, *, #3879, .F. ) ;
#4931 = FACE_OUTER_BOUND ( 'NONE', #149, .T. ) ;
#4932 = CARTESIAN_POINT ( 'NONE',  ( -85.74999999999981526, 15.00000000000010836, 10.00000000000017586 ) ) ;
#4933 = CARTESIAN_POINT ( 'NONE',  ( -335.0000000000001137, 80.00000000000001421, 50.00000000000001421 ) ) ;
#4934 = ORIENTED_EDGE ( 'NONE', *, *, #6341, .T. ) ;
#4935 = FACE_OUTER_BOUND ( 'NONE', #4526, .T. ) ;
#4936 = EDGE_LOOP ( 'NONE', ( #726, #887 ) ) ;
#4937 = CARTESIAN_POINT ( 'NONE',  ( 10.00000000000000888, -650.0000000000002274, 79.99999999999995737 ) ) ;
#4938 = EDGE_CURVE ( 'NONE', #8292, #4318, #815, .T. ) ;
#4939 = LINE ( 'NONE', #4285, #2542 ) ;
#4940 = DIRECTION ( 'NONE',  ( -3.851859888774471706E-33, 7.598173571352223877E-18, -1.000000000000000000 ) ) ;
#4941 = ORIENTED_EDGE ( 'NONE', *, *, #4629, .T. ) ;
#4942 = LINE ( 'NONE', #5478, #8214 ) ;
#4943 = ORIENTED_EDGE ( 'NONE', *, *, #5928, .F. ) ;
#4944 = ORIENTED_EDGE ( 'NONE', *, *, #3430, .T. ) ;
#4945 = CARTESIAN_POINT ( 'NONE',  ( 3.318518101603081139, 7.321656987762871438, -8.400000000000003908 ) ) ;
#4946 = EDGE_CURVE ( 'NONE', #4181, #3380, #801, .T. ) ;
#4947 = AXIS2_PLACEMENT_3D ( 'NONE', #7179, #7704, #4399 ) ;
#4948 = LINE ( 'NONE', #6714, #941 ) ;
#4949 = CARTESIAN_POINT ( 'NONE',  ( 4.000000000000225597, -6.928203230275542523, -8.400000000000018119 ) ) ;
#4950 = B_SPLINE_CURVE_WITH_KNOTS ( 'NONE', 3,
 ( #1950, #1295, #7305, #3995, #6658, #7515 ),
 .UNSPECIFIED., .F., .F.,
 ( 4, 2, 4 ),
 ( 2.380731626811020739E-07, 0.002336973833157370787, 0.004673709593152060304 ),
 .UNSPECIFIED. ) ;
#4951 = FACE_OUTER_BOUND ( 'NONE', #7721, .T. ) ;
#4952 = CARTESIAN_POINT ( 'NONE',  ( 4.000000000000003553, 2.639212418033096252, 1.523750000000267946 ) ) ;
#4953 = CARTESIAN_POINT ( 'NONE',  ( 8.000000000000007105, -4.618802153517121312, -7.685468820183672278 ) ) ;
#4954 = LINE ( 'NONE', #7774, #3967 ) ;
#4955 = ORIENTED_EDGE ( 'NONE', *, *, #7992, .F. ) ;
#4956 = ORIENTED_EDGE ( 'NONE', *, *, #4434, .F. ) ;
#4957 = AXIS2_PLACEMENT_3D ( 'NONE', #2859, #6874, #6186 ) ;
#4958 = ADVANCED_FACE ( 'NONE', ( #789 ), #6494, .T. ) ;
#4959 = DIRECTION ( 'NONE',  ( 0.000000000000000000, 0.000000000000000000, -1.000000000000000000 ) ) ;
#4960 = VECTOR ( 'NONE', #1981, 1000.000000000000000 ) ;
#4961 = EDGE_CURVE ( 'NONE', #1663, #7727, #6806, .T. ) ;
#4962 = LINE ( 'NONE', #4269, #5546 ) ;
#4963 = EDGE_LOOP ( 'NONE', ( #5124, #4941, #6929, #940 ) ) ;
#4964 = ORIENTED_EDGE ( 'NONE', *, *, #6889, .T. ) ;
#4965 = VECTOR ( 'NONE', #8109, 1000.000000000000227 ) ;
#4966 = DIRECTION ( 'NONE',  ( 0.000000000000000000, 0.000000000000000000, -1.000000000000000000 ) ) ;
#4967 = PLANE ( 'NONE',  #4061 ) ;
#4968 = LINE ( 'NONE', #7629, #966 ) ;
#4969 = ORIENTED_EDGE ( 'NONE', *, *, #5664, .T. ) ;
#4970 = DIRECTION ( 'NONE',  ( 0.000000000000000000, 0.000000000000000000, -1.000000000000000000 ) ) ;
#4971 = DIRECTION ( 'NONE',  ( 1.000000000000000000, 8.881784197001244435E-16, 0.000000000000000000 ) ) ;
#4972 = CARTESIAN_POINT ( 'NONE',  ( -422.5000000000002274, 30.00000000000002842, 68.00000000000000000 ) ) ;
#4973 = ORIENTED_EDGE ( 'NONE', *, *, #5145, .F. ) ;
#4974 = CARTESIAN_POINT ( 'NONE',  ( 0.000000000000000000, -299.9999999999999432, 0.000000000000000000 ) ) ;
#4975 = VERTEX_POINT ( 'NONE', #6159 ) ;
#4976 = DIRECTION ( 'NONE',  ( 6.400024471207000214E-36, -1.000000000000000000, 0.000000000000000000 ) ) ;
#4977 = CARTESIAN_POINT ( 'NONE',  ( 0.000000000000000000, 0.000000000000000000, -50.00000000000000000 ) ) ;
#4978 = ORIENTED_EDGE ( 'NONE', *, *, #6832, .T. ) ;
#4979 = FACE_OUTER_BOUND ( 'NONE', #6769, .T. ) ;
#4980 = TOROIDAL_SURFACE ( 'NONE', #821, 4.400000000000030553, 0.4000000000000000222 ) ;
#4981 = ORIENTED_EDGE ( 'NONE', *, *, #1321, .T. ) ;
#4982 = EDGE_CURVE ( 'NONE', #6245, #4565, #384, .T. ) ;
#4983 = LINE ( 'NONE', #378, #6564 ) ;
#4984 = ORIENTED_EDGE ( 'NONE', *, *, #27, .T. ) ;
#4985 = DIRECTION ( 'NONE',  ( 0.000000000000000000, 0.000000000000000000, -1.000000000000000000 ) ) ;
#4986 = CIRCLE ( 'NONE', #2477, 15.00000000000000355 ) ;
#4987 = AXIS2_PLACEMENT_3D ( 'NONE', #1094, #5092, #7064 ) ;
#4988 = FACE_OUTER_BOUND ( 'NONE', #8110, .T. ) ;
#4989 = CARTESIAN_POINT ( 'NONE',  ( 1.110223024625156540E-13, -414.9999999999999432, -6.938893903907228378E-14 ) ) ;
#4990 = LINE ( 'NONE', #2864, #6431 ) ;
#4991 = CARTESIAN_POINT ( 'NONE',  ( 0.000000000000000000, -9.237604307034018802, -0.7145311798163467287 ) ) ;
#4992 = AXIS2_PLACEMENT_3D ( 'NONE', #5173, #2387, #5121 ) ;
#4993 = CARTESIAN_POINT ( 'NONE',  ( 0.000000000000000000, 0.000000000000000000, -50.00000000000000000 ) ) ;
#4994 = ORIENTED_EDGE ( 'NONE', *, *, #4388, .T. ) ;
#4995 = EDGE_CURVE ( 'NONE', #3689, #5847, #122, .T. ) ;
#4996 = CARTESIAN_POINT ( 'NONE',  ( 2.220446049250313081E-13, -0.8578643762688908936, -1.110223024625156540E-13 ) ) ;
#4997 = ORIENTED_EDGE ( 'NONE', *, *, #133, .T. ) ;
#4998 = CARTESIAN_POINT ( 'NONE',  ( -275.0000000000000000, 425.0000000000000000, 1.561424668912875158E-13 ) ) ;
#4999 = FACE_OUTER_BOUND ( 'NONE', #6807, .T. ) ;
#5000 = ORIENTED_EDGE ( 'NONE', *, *, #5598, .F. ) ;
#5001 = CIRCLE ( 'NONE', #2497, 4.171999999999999709 ) ;
#5002 = VECTOR ( 'NONE', #4779, 1000.000000000000000 ) ;
#5003 = ORIENTED_EDGE ( 'NONE', *, *, #1062, .T. ) ;
#5004 = ADVANCED_FACE ( 'NONE', ( #1947 ), #5215, .T. ) ;
#5005 = AXIS2_PLACEMENT_3D ( 'NONE', #4306, #3657, #1513 ) ;
#5006 = CIRCLE ( 'NONE', #1951, 8.000000000000007105 ) ;
#5007 = VECTOR ( 'NONE', #4407, 1000.000000000000000 ) ;
#5008 = PRODUCT_DEFINITION_SHAPE ( 'NONE', 'NONE',  #8627 ) ;
#5009 = B_SPLINE_CURVE_WITH_KNOTS ( 'NONE', 3,
 ( #3285, #725, #6015, #2772, #5967, #99, #6697, #6 ),
 .UNSPECIFIED., .F., .F.,
 ( 4, 2, 2, 4 ),
 ( 0.004673709593151410650, 0.005837709341827138597, 0.007001709090502865676, 0.009329708587854319835 ),
 .UNSPECIFIED. ) ;
#5010 = CARTESIAN_POINT ( 'NONE',  ( 4.000000000000003553, 1.759474945355374409, 3.047499999999869758 ) ) ;
#5011 = ORIENTED_EDGE ( 'NONE', *, *, #3031, .T. ) ;
#5012 = CARTESIAN_POINT ( 'NONE',  ( 139.9999999999994316, 3.469446951953611664E-14, 4.171999999998556419 ) ) ;
#5013 = DIRECTION ( 'NONE',  ( 1.000000000000000000, 2.775557561562914622E-15, -3.821045009664285041E-30 ) ) ;
#5014 = APPLICATION_PROTOCOL_DEFINITION ( 'draft international standard', 'automotive_design', 1998, #8190 ) ;
#5015 = CIRCLE ( 'NONE', #6421, 8.000000000000007105 ) ;
#5016 = EDGE_CURVE ( 'NONE', #2290, #3126, #5537, .T. ) ;
#5017 = PLANE ( 'NONE',  #3480 ) ;
#5018 = DIRECTION ( 'NONE',  ( 0.000000000000000000, 0.000000000000000000, 1.000000000000000000 ) ) ;
#5019 = ADVANCED_FACE ( 'NONE', ( #3992 ), #1075, .T. ) ;
#5020 = DIRECTION ( 'NONE',  ( 0.000000000000000000, 0.000000000000000000, 1.000000000000000000 ) ) ;
#5021 = ORIENTED_EDGE ( 'NONE', *, *, #5408, .T. ) ;
#5022 = FACE_OUTER_BOUND ( 'NONE', #5785, .T. ) ;
#5023 = ORIENTED_EDGE ( 'NONE', *, *, #7992, .T. ) ;
#5024 = ORIENTED_EDGE ( 'NONE', *, *, #6539, .F. ) ;
#5025 = DIRECTION ( 'NONE',  ( 6.938893903907228378E-17, 0.000000000000000000, 1.000000000000000000 ) ) ;
#5026 = ORIENTED_EDGE ( 'NONE', *, *, #4549, .T. ) ;
#5027 = FACE_OUTER_BOUND ( 'NONE', #4395, .T. ) ;
#5028 = CARTESIAN_POINT ( 'NONE',  ( -2.300000000000024247, 0.000000000000000000, 10.00000000000000178 ) ) ;
#5029 = AXIS2_PLACEMENT_3D ( 'NONE', #6363, #8394, #387 ) ;
#5030 = DIRECTION ( 'NONE',  ( 1.000000000000000000, 8.881784197001244435E-16, 0.000000000000000000 ) ) ;
#5031 = ADVANCED_FACE ( 'NONE', ( #2560 ), #2190, .F. ) ;
#5032 =( LENGTH_UNIT ( ) NAMED_UNIT ( * ) SI_UNIT ( .MILLI., .METRE. ) );
#5033 = VECTOR ( 'NONE', #7712, 1000.000000000000000 ) ;
#5034 = DIRECTION ( 'NONE',  ( -0.000000000000000000, -0.000000000000000000, 1.000000000000000000 ) ) ;
#5035 = CARTESIAN_POINT ( 'NONE',  ( 32.49999999999997158, 1.387778780781445676E-14, 0.000000000000000000 ) ) ;
#5036 = CARTESIAN_POINT ( 'NONE',  ( -31.74999999999994316, 0.000000000000000000, 0.000000000000000000 ) ) ;
#5037 = ORIENTED_EDGE ( 'NONE', *, *, #1498, .T. ) ;
#5038 = PLANE ( 'NONE',  #2926 ) ;
#5039 = ORIENTED_EDGE ( 'NONE', *, *, #2113, .T. ) ;
#5040 = ADVANCED_FACE ( 'NONE', ( #2033 ), #1242, .T. ) ;
#5041 = CONICAL_SURFACE ( 'NONE', #6721, 50.00000000000008527, 0.7853981633974497223 ) ;
#5042 = CYLINDRICAL_SURFACE ( 'NONE', #6471, 25.00000000000000711 ) ;
#5043 = EDGE_CURVE ( 'NONE', #4558, #3833, #5895, .T. ) ;
#5044 = DIRECTION ( 'NONE',  ( 1.000000000000000000, 2.715219353702835081E-15, 0.000000000000000000 ) ) ;
#5045 = B_SPLINE_CURVE_WITH_KNOTS ( 'NONE', 3,
 ( #4080, #2735, #5390, #8089, #6828, #8043, #6745, #3470 ),
 .UNSPECIFIED., .F., .F.,
 ( 4, 2, 2, 4 ),
 ( 0.004673709593152062039, 0.005837709341827626922, 0.007001709090503191804, 0.009329708587854326773 ),
 .UNSPECIFIED. ) ;
#5046 = CIRCLE ( 'NONE', #3526, 5.500000000000000000 ) ;
#5047 = ORIENTED_EDGE ( 'NONE', *, *, #3765, .F. ) ;
#5048 = CARTESIAN_POINT ( 'NONE',  ( 8.000000000000007105, 4.618802153516732290, -7.685468820183672278 ) ) ;
#5049 = CIRCLE ( 'NONE', #4787, 75.00000000000000000 ) ;
#5050 = UNCERTAINTY_MEASURE_WITH_UNIT (LENGTH_MEASURE( 1.000000000000000082E-05 ), #3688, 'distance_accuracy_value', 'NONE');
#5051 = CIRCLE ( 'NONE', #479, 15.00000000000000355 ) ;
#5052 = EDGE_CURVE ( 'NONE', #5649, #8044, #6376, .T. ) ;
#5053 = CIRCLE ( 'NONE', #5782, 4.499999999999997335 ) ;
#5054 = CARTESIAN_POINT ( 'NONE',  ( -34.99999999999963052, 120.0000000000003695, 9.999999999999980460 ) ) ;
#5055 = DIRECTION ( 'NONE',  ( 0.000000000000000000, 0.000000000000000000, 1.000000000000000000 ) ) ;
#5056 = ORIENTED_EDGE ( 'NONE', *, *, #3146, .F. ) ;
#5057 = CARTESIAN_POINT ( 'NONE',  ( 4.680456609904033449, 6.535341423375591319, -8.383111142572232666 ) ) ;
#5058 = CARTESIAN_POINT ( 'NONE',  ( -3.999999999999892530, 6.928203230275431501, -8.400000000000018119 ) ) ;
#5059 = CARTESIAN_POINT ( 'NONE',  ( -487.5000000000002842, 30.00000000000006750, 67.99999999999998579 ) ) ;
#5060 =( REPRESENTATION_RELATIONSHIP ('NONE','NONE', #1279, #6969 ) REPRESENTATION_RELATIONSHIP_WITH_TRANSFORMATION ( #4748 )SHAPE_REPRESENTATION_RELATIONSHIP( ) );
#5061 = LINE ( 'NONE', #7638, #6726 ) ;
#5062 = EDGE_CURVE ( 'NONE', #6954, #7534, #550, .T. ) ;
#5063 = ORIENTED_EDGE ( 'NONE', *, *, #7094, .F. ) ;
#5064 = DIRECTION ( 'NONE',  ( 0.000000000000000000, 0.000000000000000000, 1.000000000000000000 ) ) ;
#5065 = CARTESIAN_POINT ( 'NONE',  ( -99.99999999999972999, 0.000000000000000000, 9.999999999999980460 ) ) ;
#5066 = CARTESIAN_POINT ( 'NONE',  ( -8.000000000000229150, 4.618802153516954334, -0.7145311798163467287 ) ) ;
#5067 =( NAMED_UNIT ( * ) SI_UNIT ( $, .STERADIAN. ) SOLID_ANGLE_UNIT ( ) );
#5068 = ORIENTED_EDGE ( 'NONE', *, *, #856, .T. ) ;
#5069 = CARTESIAN_POINT ( 'NONE',  ( 0.000000000000000000, 0.000000000000000000, -8.400000000000018119 ) ) ;
#5070 = ORIENTED_EDGE ( 'NONE', *, *, #5507, .F. ) ;
#5071 = VECTOR ( 'NONE', #7022, 1000.000000000000000 ) ;
#5072 = DIRECTION ( 'NONE',  ( -1.000000000000000000, 0.000000000000000000, -6.938893903907228378E-17 ) ) ;
#5073 = EDGE_CURVE ( 'NONE', #2801, #3286, #3168, .T. ) ;
#5074 = LINE ( 'NONE', #7729, #3013 ) ;
#5075 = PLANE ( 'NONE',  #1140 ) ;
#5076 = CARTESIAN_POINT ( 'NONE',  ( 8.000000000000012434, 0.7809653281576679484, -5.991911068876919021E-15 ) ) ;
#5077 = CARTESIAN_POINT ( 'NONE',  ( 2.220446049250313081E-13, 9.237604307034075646, -7.685468820183672278 ) ) ;
#5078 = VERTEX_POINT ( 'NONE', #597 ) ;
#5079 = ORIENTED_EDGE ( 'NONE', *, *, #7102, .F. ) ;
#5080 = ADVANCED_FACE ( 'NONE', ( #1379 ), #4438, .T. ) ;
#5081 = CARTESIAN_POINT ( 'NONE',  ( 2.645508037661675083, 7.710219529346487910, -0.06809871960532241919 ) ) ;
#5082 = CONTEXT_DEPENDENT_SHAPE_REPRESENTATION ( #4127, #5509 ) ;
#5083 = ORIENTED_EDGE ( 'NONE', *, *, #402, .F. ) ;
#5084 = CARTESIAN_POINT ( 'NONE',  ( 0.000000000000000000, 0.000000000000000000, 0.000000000000000000 ) ) ;
#5085 = ORIENTED_EDGE ( 'NONE', *, *, #98, .T. ) ;
#5086 = ORIENTED_EDGE ( 'NONE', *, *, #7702, .F. ) ;
#5087 = CARTESIAN_POINT ( 'NONE',  ( -6.661338147750939243E-13, 9.237604307034352757, -7.685468820183672278 ) ) ;
#5088 = AXIS2_PLACEMENT_3D ( 'NONE', #7434, #1465, #6145 ) ;
#5089 = EDGE_CURVE ( 'NONE', #7453, #1219, #6123, .T. ) ;
#5090 = AXIS2_PLACEMENT_3D ( 'NONE', #1807, #4464, #7126 ) ;
#5091 = CARTESIAN_POINT ( 'NONE',  ( 8.000000000000238032, -3.867591403079324142, -0.4976753153247437944 ) ) ;
#5092 = DIRECTION ( 'NONE',  ( 0.000000000000000000, 0.000000000000000000, 1.000000000000000000 ) ) ;
#5093 = VERTEX_POINT ( 'NONE', #5163 ) ;
#5094 = CARTESIAN_POINT ( 'NONE',  ( -4.000000000000003553, 6.928203230275431501, 0.000000000000000000 ) ) ;
#5095 = DIRECTION ( 'NONE',  ( -3.851859888774471706E-33, 7.598173571352219255E-18, -1.000000000000000000 ) ) ;
#5096 = CARTESIAN_POINT ( 'NONE',  ( 2.309976723937089194, -7.903938623646893369, -8.269346954796276350 ) ) ;
#5097 = PRODUCT_CONTEXT ( 'NONE', #1468, 'mechanical' ) ;
#5098 = ADVANCED_FACE ( 'NONE', ( #8557 ), #4587, .T. ) ;
#5099 = FACE_OUTER_BOUND ( 'NONE', #6781, .T. ) ;
#5100 = EDGE_LOOP ( 'NONE', ( #5495, #6333, #4766, #1683, #965 ) ) ;
#5101 = CARTESIAN_POINT ( 'NONE',  ( 10.00000000000000888, 9.797174393176348634E-16, -7.999999999999555911 ) ) ;
#5102 = DIRECTION ( 'NONE',  ( 0.000000000000000000, -4.930380657631255821E-30, 1.000000000000000000 ) ) ;
#5103 = SHAPE_REPRESENTATION_RELATIONSHIP ( 'NONE' , 'NONE' ,  #3167, #212 ) ;
#5104 = VERTEX_POINT ( 'NONE', #3340 ) ;
#5105 = EDGE_CURVE ( 'NONE', #6936, #4831, #1235, .T. ) ;
#5106 = LINE ( 'NONE', #1149, #2137 ) ;
#5107 = ORIENTED_EDGE ( 'NONE', *, *, #4840, .T. ) ;
#5108 = CARTESIAN_POINT ( 'NONE',  ( -7.347286611336937945, -4.995646404165699828, -0.4969600502618697346 ) ) ;
#5109 = FACE_OUTER_BOUND ( 'NONE', #6465, .T. ) ;
#5110 = DIRECTION ( 'NONE',  ( -3.919652622816902408E-30, -3.944304526105059027E-30, 1.000000000000000000 ) ) ;
#5111 = LINE ( 'NONE', #1041, #8223 ) ;
#5112 = CARTESIAN_POINT ( 'NONE',  ( 4.898587196589422492E-15, -40.00000000000007816, -3.039269428540890907E-16 ) ) ;
#5113 = EDGE_CURVE ( 'NONE', #6426, #3965, #9, .T. ) ;
#5114 = CARTESIAN_POINT ( 'NONE',  ( 8.000000000000007105, 4.618802153517065356, -0.7145311798163467287 ) ) ;
#5115 = CARTESIAN_POINT ( 'NONE',  ( 8.000000000000012434, -1.555946510856071940, -8.332911297836661291 ) ) ;
#5116 = ORIENTED_EDGE ( 'NONE', *, *, #3145, .F. ) ;
#5117 = CYLINDRICAL_SURFACE ( 'NONE', #6686, 14.99999999999986677 ) ;
#5118 = ORIENTED_EDGE ( 'NONE', *, *, #6846, .T. ) ;
#5119 = CARTESIAN_POINT ( 'NONE',  ( 8.000000000000008882, 3.871967595402188156, -7.901061386767544548 ) ) ;
#5120 = ADVANCED_FACE ( 'NONE', ( #8516 ), #7909, .F. ) ;
#5121 = DIRECTION ( 'NONE',  ( 6.400024471206996205E-36, -1.000000000000000000, -7.598173571352216173E-18 ) ) ;
#5122 = EDGE_LOOP ( 'NONE', ( #1751, #3226, #7039, #6783 ) ) ;
#5123 = VECTOR ( 'NONE', #1723, 1000.000000000000000 ) ;
#5124 = ORIENTED_EDGE ( 'NONE', *, *, #7145, .F. ) ;
#5125 = FACE_OUTER_BOUND ( 'NONE', #8365, .T. ) ;
#5126 = ORIENTED_EDGE ( 'NONE', *, *, #2924, .F. ) ;
#5127 = AXIS2_PLACEMENT_3D ( 'NONE', #3509, #903, #6873 ) ;
#5128 = AXIS2_PLACEMENT_3D ( 'NONE', #2734, #1939, #7252 ) ;
#5129 = DIRECTION ( 'NONE',  ( -3.851859888774464864E-33, 1.232595164407830946E-32, 1.000000000000000000 ) ) ;
#5130 = AXIS2_PLACEMENT_3D ( 'NONE', #3596, #4244, #7510 ) ;
#5131 = DIRECTION ( 'NONE',  ( 0.000000000000000000, 0.000000000000000000, 1.000000000000000000 ) ) ;
#5132 = FILL_AREA_STYLE ('',( #1965 ) ) ;
#5133 = EDGE_CURVE ( 'NONE', #4033, #5923, #6516, .T. ) ;
#5134 = EDGE_LOOP ( 'NONE', ( #6016, #3927 ) ) ;
#5135 = CARTESIAN_POINT ( 'NONE',  ( -3.999999999999781508, -6.928203230275875590, -8.400000000000018119 ) ) ;
#5136 = AXIS2_PLACEMENT_3D ( 'NONE', #5466, #929, #6255 ) ;
#5137 = VECTOR ( 'NONE', #5313, 1000.000000000000000 ) ;
#5138 = LINE ( 'NONE', #3760, #6411 ) ;
#5139 = CIRCLE ( 'NONE', #8485, 5.500000000000000000 ) ;
#5140 = DIRECTION ( 'NONE',  ( -1.000000000000000000, -8.881784197001244435E-16, 0.000000000000000000 ) ) ;
#5141 = CARTESIAN_POINT ( 'NONE',  ( -455.0000000000003979, -2.499999999999946709, 67.99999999999994316 ) ) ;
#5142 = PRESENTATION_LAYER_ASSIGNMENT (  '', '', ( #3893 ) ) ;
#5143 = B_SPLINE_CURVE_WITH_KNOTS ( 'NONE', 3,
 ( #3986, #55, #7337, #2685, #5344, #3374 ),
 .UNSPECIFIED., .F., .F.,
 ( 4, 2, 4 ),
 ( 0.01291313371729494071, 0.01525081363757336758, 0.01758849355785179619 ),
 .UNSPECIFIED. ) ;
#5144 = CONICAL_SURFACE ( 'NONE', #6287, 8.000000000000007105, 1.047197551196597631 ) ;
#5145 = EDGE_CURVE ( 'NONE', #5698, #5867, #3290, .T. ) ;
#5146 = DIRECTION ( 'NONE',  ( 3.919652622816902408E-30, 3.944304526105059027E-30, -1.000000000000000000 ) ) ;
#5147 = EDGE_CURVE ( 'NONE', #5920, #5838, #2356, .T. ) ;
#5148 = ORIENTED_EDGE ( 'NONE', *, *, #2191, .F. ) ;
#5149 = CARTESIAN_POINT ( 'NONE',  ( 2.220446049250313081E-13, 9.237604307034075646, -8.400000000000018119 ) ) ;
#5150 = ORIENTED_EDGE ( 'NONE', *, *, #5089, .F. ) ;
#5151 = CARTESIAN_POINT ( 'NONE',  ( 4.000000000000003553, -3.518949890710769690, 0.000000000000000000 ) ) ;
#5152 = VERTEX_POINT ( 'NONE', #4892 ) ;
#5153 = CARTESIAN_POINT ( 'NONE',  ( 4.000000000000058620, 3.518949890710762585, 2.220446049250313081E-13 ) ) ;
#5154 = PRODUCT_DEFINITION_CONTEXT ( 'detailed design', #6215, 'design' ) ;
#5155 = CARTESIAN_POINT ( 'NONE',  ( 33.00000000000055422, -1.431146867680865853E-14, 6.883382752675970551E-12 ) ) ;
#5156 = EDGE_CURVE ( 'NONE', #4220, #7819, #2919, .T. ) ;
#5157 = FILL_AREA_STYLE_COLOUR ( '', #5745 ) ;
#5158 = CARTESIAN_POINT ( 'NONE',  ( -1.313474075707240729, -8.479269695850863542, -0.3167204509598423590 ) ) ;
#5159 = DIRECTION ( 'NONE',  ( 1.000000000000000000, 0.000000000000000000, 0.000000000000000000 ) ) ;
#5160 = CARTESIAN_POINT ( 'NONE',  ( 0.000000000000000000, 0.000000000000000000, 0.000000000000000000 ) ) ;
#5161 = ORIENTED_EDGE ( 'NONE', *, *, #3255, .T. ) ;
#5162 = ORIENTED_EDGE ( 'NONE', *, *, #8047, .T. ) ;
#5163 = CARTESIAN_POINT ( 'NONE',  ( 7.999999999999340972, -4.618802153516732290, -7.685468820183672278 ) ) ;
#5164 = AXIS2_PLACEMENT_3D ( 'NONE', #1597, #8024, #1674 ) ;
#5165 = ADVANCED_FACE ( 'NONE', ( #8251 ), #368, .F. ) ;
#5166 = ADVANCED_FACE ( 'NONE', ( #5606 ), #6994, .F. ) ;
#5167 =( LENGTH_UNIT ( ) NAMED_UNIT ( * ) SI_UNIT ( .MILLI., .METRE. ) );
#5168 = CONICAL_SURFACE ( 'NONE', #6563, 8.000000000000007105, 1.047197551196597631 ) ;
#5169 = PLANE ( 'NONE',  #1163 ) ;
#5170 = CONTEXT_DEPENDENT_SHAPE_REPRESENTATION ( #7125, #2095 ) ;
#5171 = ORIENTED_EDGE ( 'NONE', *, *, #4480, .T. ) ;
#5172 = B_SPLINE_CURVE_WITH_KNOTS ( 'NONE', 3,
 ( #5882, #8504, #4420, #7726, #2545, #8543 ),
 .UNSPECIFIED., .F., .F.,
 ( 4, 2, 4 ),
 ( 2.380731628162083024E-07, 0.002336973833157790156, 0.004673709593152763735 ),
 .UNSPECIFIED. ) ;
#5173 = CARTESIAN_POINT ( 'NONE',  ( 0.000000000000000000, 0.000000000000000000, 130.0000000000000000 ) ) ;
#5174 = ORIENTED_EDGE ( 'NONE', *, *, #8192, .F. ) ;
#5175 = CARTESIAN_POINT ( 'NONE',  ( 0.000000000000000000, 0.000000000000000000, 0.000000000000000000 ) ) ;
#5176 = VERTEX_POINT ( 'NONE', #6304 ) ;
#5177 = VECTOR ( 'NONE', #7755, 1000.000000000000000 ) ;
#5178 = CARTESIAN_POINT ( 'NONE',  ( -4.440892098500626162E-13, -9.237604307034018802, -7.685468820183672278 ) ) ;
#5179 = EDGE_CURVE ( 'NONE', #1467, #3109, #7367, .T. ) ;
#5180 = EDGE_CURVE ( 'NONE', #4232, #922, #7512, .T. ) ;
#5181 = CARTESIAN_POINT ( 'NONE',  ( -50.00000000000004263, -500.0000000000000000, -50.00000000000000000 ) ) ;
#5182 = DIRECTION ( 'NONE',  ( 0.000000000000000000, 0.000000000000000000, 1.000000000000000000 ) ) ;
#5183 = AXIS2_PLACEMENT_3D ( 'NONE', #3310, #125, #2794 ) ;
#5184 = DIRECTION ( 'NONE',  ( 0.000000000000000000, 0.000000000000000000, 1.000000000000000000 ) ) ;
#5185 = DIRECTION ( 'NONE',  ( -1.000000000000000000, 1.774937036747276562E-30, 0.000000000000000000 ) ) ;
#5186 = EDGE_LOOP ( 'NONE', ( #6163, #7686, #6526, #5941 ) ) ;
#5187 = CARTESIAN_POINT ( 'NONE',  ( -2.645508037661987277, -7.710219529346969303, -8.331901280394371057 ) ) ;
#5188 = APPLICATION_CONTEXT ( 'automotive_design' ) ;
#5189 = AXIS2_PLACEMENT_3D ( 'NONE', #3732, #5718, #6396 ) ;
#5190 = B_SPLINE_CURVE_WITH_KNOTS ( 'NONE', 3,
 ( #4491, #7677, #4369, #1180, #5096, #4451, #7031, #1097 ),
 .UNSPECIFIED., .F., .F.,
 ( 4, 2, 2, 4 ),
 ( 0.004673709593152784551, 0.005837709341828078817, 0.007001709090503373950, 0.009329708587853959012 ),
 .UNSPECIFIED. ) ;
#5191 = ADVANCED_FACE ( 'NONE', ( #3017 ), #5017, .F. ) ;
#5192 = AXIS2_PLACEMENT_3D ( 'NONE', #7149, #1172, #3307 ) ;
#5193 = VECTOR ( 'NONE', #6792, 1000.000000000000000 ) ;
#5194 = CARTESIAN_POINT ( 'NONE',  ( 4.000000000000225597, -6.928203230275542523, -8.400000000000018119 ) ) ;
#5195 = ORIENTED_EDGE ( 'NONE', *, *, #4901, .F. ) ;
#5196 = CIRCLE ( 'NONE', #5642, 8.000000000000000000 ) ;
#5197 = CARTESIAN_POINT ( 'NONE',  ( 4.000000000000003553, 1.759474945355415931, -3.047500000000091802 ) ) ;
#5198 =( NAMED_UNIT ( * ) SI_UNIT ( $, .STERADIAN. ) SOLID_ANGLE_UNIT ( ) );
#5199 = ORIENTED_EDGE ( 'NONE', *, *, #8411, .F. ) ;
#5200 = AXIS2_PLACEMENT_3D ( 'NONE', #6257, #1831, #7800 ) ;
#5201 = FACE_OUTER_BOUND ( 'NONE', #4218, .T. ) ;
#5202 = ORIENTED_EDGE ( 'NONE', *, *, #5179, .T. ) ;
#5203 = FACE_OUTER_BOUND ( 'NONE', #7101, .T. ) ;
#5204 = EDGE_CURVE ( 'NONE', #181, #8316, #7650, .T. ) ;
#5205 = FACE_OUTER_BOUND ( 'NONE', #6862, .T. ) ;
#5206 = CARTESIAN_POINT ( 'NONE',  ( 4.059252933785728601E-13, 119.9999999999998863, 0.000000000000000000 ) ) ;
#5207 = DIRECTION ( 'NONE',  ( 6.400024471206997542E-36, -1.000000000000000000, 0.000000000000000000 ) ) ;
#5208 = CARTESIAN_POINT ( 'NONE',  ( 2.645508037661961520, 7.710219529346607814, -0.06809871960544289227 ) ) ;
#5209 = SHAPE_REPRESENTATION ( 'Conveyor belt', ( #7563 ), #1574 ) ;
#5210 = CARTESIAN_POINT ( 'NONE',  ( 0.000000000000000000, -1.759474945355374631, 3.047500000000091802 ) ) ;
#5211 = CARTESIAN_POINT ( 'NONE',  ( 8.000000000000015987, -3.098204225878034901, -8.084209322808163733 ) ) ;
#5212 = ORIENTED_EDGE ( 'NONE', *, *, #254, .F. ) ;
#5213 = SURFACE_STYLE_USAGE ( .BOTH. , #3206 ) ;
#5214 = EDGE_LOOP ( 'NONE', ( #5680, #7409, #3065, #6663 ) ) ;
#5215 = PLANE ( 'NONE',  #4698 ) ;
#5216 = ADVANCED_FACE ( 'NONE', ( #4935 ), #3680, .F. ) ;
#5217 = CARTESIAN_POINT ( 'NONE',  ( 8.000000000000234479, -1.555946510856276666, -8.332911297836512077 ) ) ;
#5218 = PRODUCT ( 'MAT-028', 'MAT-028', '', ( #5747 ) ) ;
#5219 = CARTESIAN_POINT ( 'NONE',  ( 3.000384657911011130E-15, 299.9999999999999432, -24.50000000000007461 ) ) ;
#5220 = ORIENTED_EDGE ( 'NONE', *, *, #2321, .T. ) ;
#5221 = CARTESIAN_POINT ( 'NONE',  ( 44.99999999999992895, -500.0000000000000000, -45.00000000000000711 ) ) ;
#5222 = ORIENTED_EDGE ( 'NONE', *, *, #7748, .T. ) ;
#5223 = VECTOR ( 'NONE', #1551, 1000.000000000000000 ) ;
#5224 = EDGE_LOOP ( 'NONE', ( #4856, #5475, #2442, #4934 ) ) ;
#5225 = EDGE_CURVE ( 'NONE', #367, #4193, #7781, .T. ) ;
#5226 = CARTESIAN_POINT ( 'NONE',  ( -2.645508037661928213, -7.710219529346594491, -8.331901280394589548 ) ) ;
#5227 = VERTEX_POINT ( 'NONE', #935 ) ;
#5228 = DIRECTION ( 'NONE',  ( -3.851859888774471706E-33, 7.598173571352219255E-18, -1.000000000000000000 ) ) ;
#5229 = CARTESIAN_POINT ( 'NONE',  ( -8.000000000000229150, -4.618802153516843312, -7.685468820183672278 ) ) ;
#5230 = CARTESIAN_POINT ( 'NONE',  ( 2.388061258337334995E-15, 415.0000000000000000, 19.49999999999991473 ) ) ;
#5231 = SURFACE_STYLE_USAGE ( .BOTH. , #7887 ) ;
#5232 = EDGE_LOOP ( 'NONE', ( #7674, #7645, #3603, #1129 ) ) ;
#5233 = CIRCLE ( 'NONE', #221, 8.000000000000007105 ) ;
#5234 = DIRECTION ( 'NONE',  ( -3.919652622816902408E-30, -3.944304526105059027E-30, 1.000000000000000000 ) ) ;
#5235 = EDGE_CURVE ( 'NONE', #5227, #8055, #5001, .T. ) ;
#5236 = APPLICATION_PROTOCOL_DEFINITION ( 'draft international standard', 'automotive_design', 1998, #2345 ) ;
#5237 = SURFACE_STYLE_FILL_AREA ( #6925 ) ;
#5238 = AXIS2_PLACEMENT_3D ( 'NONE', #7168, #1719, #2460 ) ;
#5239 = ORIENTED_EDGE ( 'NONE', *, *, #47, .T. ) ;
#5240 = DIRECTION ( 'NONE',  ( 0.000000000000000000, -1.042965139114318396E-29, 1.000000000000000000 ) ) ;
#5241 = EDGE_CURVE ( 'NONE', #8027, #5503, #3755, .T. ) ;
#5242 = VECTOR ( 'NONE', #5305, 1000.000000000000227 ) ;
#5243 =( LENGTH_UNIT ( ) NAMED_UNIT ( * ) SI_UNIT ( .MILLI., .METRE. ) );
#5244 = ORIENTED_EDGE ( 'NONE', *, *, #1872, .T. ) ;
#5245 = CARTESIAN_POINT ( 'NONE',  ( -14.24999999999986855, 15.00000000000014211, 2.234078735489191628E-29 ) ) ;
#5246 = EDGE_LOOP ( 'NONE', ( #1365, #1347, #7194, #6728 ) ) ;
#5247 = DIRECTION ( 'NONE',  ( 3.549874073494553124E-30, -0.5000000000000009992, -0.8660254037844380415 ) ) ;
#5248 = PRODUCT_DEFINITION_CONTEXT ( 'detailed design', #3239, 'design' ) ;
#5249 = CARTESIAN_POINT ( 'NONE',  ( 5.080504117408896292, 2.106769544347820933, -8.401000000000047763 ) ) ;
#5250 = LINE ( 'NONE', #679, #1233 ) ;
#5251 = CARTESIAN_POINT ( 'NONE',  ( -7.999999999999896083, 4.618802153516899267, -8.400000000000018119 ) ) ;
#5252 = EDGE_CURVE ( 'NONE', #369, #8044, #1699, .T. ) ;
#5253 = CARTESIAN_POINT ( 'NONE',  ( 0.000000000000000000, 60.00000000000000000, -50.00000000000000000 ) ) ;
#5254 = ORIENTED_EDGE ( 'NONE', *, *, #846, .T. ) ;
#5255 = SURFACE_SIDE_STYLE ('',( #8554 ) ) ;
#5256 = ORIENTED_EDGE ( 'NONE', *, *, #6832, .F. ) ;
#5257 = CARTESIAN_POINT ( 'NONE',  ( 0.000000000000000000, 0.000000000000000000, -8.400000000000018119 ) ) ;
#5258 = CARTESIAN_POINT ( 'NONE',  ( 4.000000000000003553, -3.518949890710769690, 0.000000000000000000 ) ) ;
#5259 = UNCERTAINTY_MEASURE_WITH_UNIT (LENGTH_MEASURE( 1.000000000000000082E-05 ), #298, 'distance_accuracy_value', 'NONE');
#5260 = CYLINDRICAL_SURFACE ( 'NONE', #5693, 15.00000000000002487 ) ;
#5261 = CYLINDRICAL_SURFACE ( 'NONE', #6353, 4.000000000000030198 ) ;
#5262 = ORIENTED_EDGE ( 'NONE', *, *, #6020, .F. ) ;
#5263 = CARTESIAN_POINT ( 'NONE',  ( 0.000000000000000000, 9.237604307034130713, -7.685468820183672278 ) ) ;
#5264 = ADVANCED_FACE ( 'NONE', ( #3384 ), #2199, .T. ) ;
#5265 = VERTEX_POINT ( 'NONE', #2236 ) ;
#5266 = ORIENTED_EDGE ( 'NONE', *, *, #8470, .T. ) ;
#5267 = DIRECTION ( 'NONE',  ( 4.622231866529366732E-33, -1.224646799147352961E-16, 1.000000000000000000 ) ) ;
#5268 = LINE ( 'NONE', #1310, #4360 ) ;
#5269 = CARTESIAN_POINT ( 'NONE',  ( -4.000000000000003553, -6.928203230275431501, -8.400000000000018119 ) ) ;
#5270 = CARTESIAN_POINT ( 'NONE',  ( 8.000000000000238032, -3.098204225878349760, -0.3157906771920377387 ) ) ;
#5271 = CARTESIAN_POINT ( 'NONE',  ( -64.99999999999940314, 120.0000000000002842, 9.999999999999980460 ) ) ;
#5272 = EDGE_LOOP ( 'NONE', ( #2775, #1600, #7986, #2203 ) ) ;
#5273 = EDGE_CURVE ( 'NONE', #2336, #4545, #6963, .T. ) ;
#5274 = CARTESIAN_POINT ( 'NONE',  ( 139.9999999999994316, 3.520539216414043934E-14, -4.172000000001442999 ) ) ;
#5275 = CONICAL_SURFACE ( 'NONE', #4288, 8.000000000000007105, 1.047197551196597631 ) ;
#5276 = CONTEXT_DEPENDENT_SHAPE_REPRESENTATION ( #2193, #4116 ) ;
#5277 = AXIS2_PLACEMENT_3D ( 'NONE', #3320, #5958, #5287 ) ;
#5278 = ADVANCED_FACE ( 'NONE', ( #1618, #4282 ), #2318, .T. ) ;
#5279 = ADVANCED_FACE ( 'NONE', ( #2034 ), #8069, .T. ) ;
#5280 = EDGE_CURVE ( 'NONE', #569, #4558, #4316, .T. ) ;
#5281 = AXIS2_PLACEMENT_3D ( 'NONE', #6900, #3499, #8247 ) ;
#5282 = AXIS2_PLACEMENT_3D ( 'NONE', #2144, #4000, #1348 ) ;
#5283 = DIRECTION ( 'NONE',  ( -1.540743955509788682E-33, -4.592425496802573602E-17, 1.000000000000000000 ) ) ;
#5284 = ORIENTED_EDGE ( 'NONE', *, *, #8095, .T. ) ;
#5285 = LINE ( 'NONE', #1971, #4320 ) ;
#5286 = CIRCLE ( 'NONE', #2105, 15.00000000000000355 ) ;
#5287 = DIRECTION ( 'NONE',  ( 1.000000000000000000, 0.000000000000000000, 0.000000000000000000 ) ) ;
#5288 = ORIENTED_EDGE ( 'NONE', *, *, #6294, .T. ) ;
#5289 = AXIS2_PLACEMENT_3D ( 'NONE', #7676, #6990, #6457 ) ;
#5290 = AXIS2_PLACEMENT_3D ( 'NONE', #3443, #2702, #5494 ) ;
#5291 = PLANE ( 'NONE',  #1984 ) ;
#5292 = ORIENTED_EDGE ( 'NONE', *, *, #4528, .T. ) ;
#5293 = LINE ( 'NONE', #4687, #7288 ) ;
#5294 = ADVANCED_FACE ( 'NONE', ( #1168, #7791 ), #1090, .F. ) ;
#5295 = PRESENTATION_LAYER_ASSIGNMENT (  '', '', ( #5303 ) ) ;
#5296 = AXIS2_PLACEMENT_3D ( 'NONE', #1272, #1885, #4682 ) ;
#5297 = DIRECTION ( 'NONE',  ( 1.000000000000000000, -1.284024588418159550E-35, 0.000000000000000000 ) ) ;
#5298 = CARTESIAN_POINT ( 'NONE',  ( -79.99999999999980105, 15.00000000000012434, 10.00000000000017586 ) ) ;
#5299 = CARTESIAN_POINT ( 'NONE',  ( 8.400000000000018119, -5.551115123125782702E-14, 6.661338147750939243E-13 ) ) ;
#5300 = FACE_OUTER_BOUND ( 'NONE', #4338, .T. ) ;
#5301 = CARTESIAN_POINT ( 'NONE',  ( 4.680456609904033449, 6.535341423375591319, -0.01688885742778744800 ) ) ;
#5302 = ORIENTED_EDGE ( 'NONE', *, *, #402, .T. ) ;
#5303=STYLED_ITEM('',(#8670),#5864);
#5304 =( LENGTH_UNIT ( ) NAMED_UNIT ( * ) SI_UNIT ( .MILLI., .METRE. ) );
#5305 = DIRECTION ( 'NONE',  ( 0.000000000000000000, 0.4999999999999986677, -0.8660254037844393737 ) ) ;
#5306 = EDGE_CURVE ( 'NONE', #5464, #5847, #7186, .T. ) ;
#5307 = DIRECTION ( 'NONE',  ( 3.851859888774471706E-33, -7.598173571352216173E-18, 1.000000000000000000 ) ) ;
#5308 = FACE_OUTER_BOUND ( 'NONE', #7333, .T. ) ;
#5309 = ITEM_DEFINED_TRANSFORMATION ( 'NONE', 'NONE', #2010,  #7563 ) ;
#5310 = CARTESIAN_POINT ( 'NONE',  ( -49.99999999999953815, 120.0000000000003268, 9.999999999999980460 ) ) ;
#5311 = DIRECTION ( 'NONE',  ( -1.774937036747276562E-30, 1.000000000000000000, -1.110768649713241713E-15 ) ) ;
#5312 = ORIENTED_EDGE ( 'NONE', *, *, #2466, .T. ) ;
#5313 = DIRECTION ( 'NONE',  ( 0.000000000000000000, 0.000000000000000000, 1.000000000000000000 ) ) ;
#5314 = ORIENTED_EDGE ( 'NONE', *, *, #2987, .T. ) ;
#5315 = CARTESIAN_POINT ( 'NONE',  ( 0.000000000000000000, -9.237604307034018802, -7.685468820183672278 ) ) ;
#5316 = CARTESIAN_POINT ( 'NONE',  ( -31.74999999999994316, 9.797174393177281462E-16, -8.000000000000000000 ) ) ;
#5317 = ADVANCED_FACE ( 'NONE', ( #6483 ), #7832, .T. ) ;
#5318 = CARTESIAN_POINT ( 'NONE',  ( 8.000000000000117240, 3.871967595402001194, -0.4989386132324870049 ) ) ;
#5319 = CIRCLE ( 'NONE', #5326, 15.00000000000000355 ) ;
#5320 = DIRECTION ( 'NONE',  ( 0.000000000000000000, 0.000000000000000000, 1.000000000000000000 ) ) ;
#5321 = CARTESIAN_POINT ( 'NONE',  ( 3.200012235603504143E-34, -50.00000000000008527, 130.0000000000000000 ) ) ;
#5322 = CARTESIAN_POINT ( 'NONE',  ( 5.000000000000004441, 0.000000000000000000, 0.000000000000000000 ) ) ;
#5323 = VERTEX_POINT ( 'NONE', #3712 ) ;
#5324 = ORIENTED_EDGE ( 'NONE', *, *, #6612, .F. ) ;
#5325 = CONICAL_SURFACE ( 'NONE', #5622, 7.000000000000000888, 0.7853981633974482790 ) ;
#5326 = AXIS2_PLACEMENT_3D ( 'NONE', #119, #3306, #7403 ) ;
#5327 = EDGE_CURVE ( 'NONE', #6269, #7120, #5777, .T. ) ;
#5328 = CARTESIAN_POINT ( 'NONE',  ( -34.92499999999998295, 0.000000000000000000, 0.000000000000000000 ) ) ;
#5329 = AXIS2_PLACEMENT_3D ( 'NONE', #8450, #2480, #5131 ) ;
#5330 = AXIS2_PLACEMENT_3D ( 'NONE', #4095, #1072, #6762 ) ;
#5331 = AXIS2_PLACEMENT_3D ( 'NONE', #4937, #3643, #1620 ) ;
#5332 = VERTEX_POINT ( 'NONE', #3750 ) ;
#5333 = CARTESIAN_POINT ( 'NONE',  ( -28.24999999999997513, 3.989921841591238568E-15, -6.938893903907228378E-15 ) ) ;
#5334 = CONICAL_SURFACE ( 'NONE', #7976, 8.000000000000007105, 1.047197551196597631 ) ;
#5335 = CARTESIAN_POINT ( 'NONE',  ( -350.0000000000001137, 0.000000000000000000, 0.000000000000000000 ) ) ;
#5336 = EDGE_LOOP ( 'NONE', ( #3452, #2773, #4460, #5646 ) ) ;
#5337 = DIRECTION ( 'NONE',  ( 6.400024471206997542E-36, -1.000000000000000000, 0.000000000000000000 ) ) ;
#5338 = VERTEX_POINT ( 'NONE', #1210 ) ;
#5339 = CIRCLE ( 'NONE', #2271, 40.00000000000007816 ) ;
#5340 = CARTESIAN_POINT ( 'NONE',  ( -4.680456609904073417, -6.535341423375602865, -0.01688885742780586036 ) ) ;
#5341 = EDGE_CURVE ( 'NONE', #7519, #1856, #2854, .T. ) ;
#5342 = EDGE_CURVE ( 'NONE', #4429, #6497, #2169, .T. ) ;
#5343 = PLANE ( 'NONE',  #6485 ) ;
#5344 = CARTESIAN_POINT ( 'NONE',  ( -8.000000000000229150, 3.871967595402047824, -0.4989386132325554501 ) ) ;
#5345 = B_SPLINE_CURVE_WITH_KNOTS ( 'NONE', 3,
 ( #434, #2556, #5211, #5115, #4394, #1239 ),
 .UNSPECIFIED., .F., .F.,
 ( 4, 2, 4 ),
 ( 0.008240550023493714918, 0.01057684187039402597, 0.01291313371729433702 ),
 .UNSPECIFIED. ) ;
#5346 = FACE_OUTER_BOUND ( 'NONE', #3492, .T. ) ;
#5347 = AXIS2_PLACEMENT_3D ( 'NONE', #1454, #6821, #7591 ) ;
#5348 = DIRECTION ( 'NONE',  ( 3.919652622816902408E-30, 3.944304526105059027E-30, -1.000000000000000000 ) ) ;
#5349 = PRESENTATION_STYLE_ASSIGNMENT (( #2693 ) ) ;
#5350 = CARTESIAN_POINT ( 'NONE',  ( 10.00000000000000888, -650.0000000000002274, 79.99999999999995737 ) ) ;
#5351 =( REPRESENTATION_RELATIONSHIP ('NONE','NONE', #1279, #6969 ) REPRESENTATION_RELATIONSHIP_WITH_TRANSFORMATION ( #7308 )SHAPE_REPRESENTATION_RELATIONSHIP( ) );
#5352 = VERTEX_POINT ( 'NONE', #3379 ) ;
#5353 = CARTESIAN_POINT ( 'NONE',  ( 8.000000000000117240, -1.110223024625156540E-13, -8.400000000000018119 ) ) ;
#5354 = FACE_OUTER_BOUND ( 'NONE', #7647, .T. ) ;
#5355 = CARTESIAN_POINT ( 'NONE',  ( 5.000000000000004441, 4.685197434473897360, 0.000000000000000000 ) ) ;
#5356 = CARTESIAN_POINT ( 'NONE',  ( -2.220446049250313081E-13, -650.0000000000000000, 79.99999999999995737 ) ) ;
#5357 = CARTESIAN_POINT ( 'NONE',  ( -4.681481898397175989, 6.534749472788146107, -8.399999999999964828 ) ) ;
#5358 = EDGE_LOOP ( 'NONE', ( #6620, #5256 ) ) ;
#5359 = EDGE_CURVE ( 'NONE', #5332, #2816, #4521, .T. ) ;
#5360 = CARTESIAN_POINT ( 'NONE',  ( 0.000000000000000000, -1.759474945355374631, 3.047500000000091802 ) ) ;
#5361 = ORIENTED_EDGE ( 'NONE', *, *, #3272, .F. ) ;
#5362 = CARTESIAN_POINT ( 'NONE',  ( -0.6543471694415565754, -8.859816792613557368, -7.903584543331262147 ) ) ;
#5363 = VERTEX_POINT ( 'NONE', #1130 ) ;
#5364 = LINE ( 'NONE', #2099, #4805 ) ;
#5365 = CIRCLE ( 'NONE', #2721, 5.500000000000023981 ) ;
#5366 = DIRECTION ( 'NONE',  ( -1.000000000000000000, 1.774937036747276562E-30, 0.000000000000000000 ) ) ;
#5367 = CARTESIAN_POINT ( 'NONE',  ( 0.000000000000000000, 0.000000000000000000, 0.000000000000000000 ) ) ;
#5368 = CARTESIAN_POINT ( 'NONE',  ( 0.000000000000000000, 299.9999999999999432, -6.938893903907228378E-14 ) ) ;
#5369 = DIRECTION ( 'NONE',  ( -1.000000000000000000, 3.549874073494553124E-30, 0.000000000000000000 ) ) ;
#5370 = ORIENTED_EDGE ( 'NONE', *, *, #643, .F. ) ;
#5371 = VERTEX_POINT ( 'NONE', #487 ) ;
#5372 = PRODUCT_DEFINITION_SHAPE ( 'NONE', 'NONE',  #8612 ) ;
#5373 = EDGE_CURVE ( 'NONE', #3489, #3348, #5365, .T. ) ;
#5374 = SURFACE_STYLE_USAGE ( .BOTH. , #8155 ) ;
#5375 = AXIS2_PLACEMENT_3D ( 'NONE', #909, #2863, #3475 ) ;
#5376 = B_SPLINE_CURVE_WITH_KNOTS ( 'NONE', 3,
 ( #7432, #1648, #1572, #3715, #6337, #3591, #2769, #4928 ),
 .UNSPECIFIED., .F., .F.,
 ( 4, 2, 2, 4 ),
 ( 0.004673709593151625756, 0.005837709341827240078, 0.007001709090502855268, 0.009329708587854083912 ),
 .UNSPECIFIED. ) ;
#5377 = DIRECTION ( 'NONE',  ( -1.000000000000000000, -3.083952846180994816E-15, 0.000000000000000000 ) ) ;
#5378 = ORIENTED_EDGE ( 'NONE', *, *, #4213, .T. ) ;
#5379 = CARTESIAN_POINT ( 'NONE',  ( 0.000000000000000000, 0.000000000000000000, 0.000000000000000000 ) ) ;
#5380 = EDGE_CURVE ( 'NONE', #7854, #4358, #7166, .T. ) ;
#5381 = ORIENTED_EDGE ( 'NONE', *, *, #5147, .F. ) ;
#5382 = CIRCLE ( 'NONE', #3435, 5.749999999999991118 ) ;
#5383 = DIRECTION ( 'NONE',  ( 0.000000000000000000, 0.000000000000000000, 1.000000000000000000 ) ) ;
#5384 = VERTEX_POINT ( 'NONE', #5087 ) ;
#5385 = CARTESIAN_POINT ( 'NONE',  ( 5.354491962337973199, -6.146186931204551840, -8.331901280394582443 ) ) ;
#5386 = CIRCLE ( 'NONE', #1199, 4.250000000000010658 ) ;
#5387 = FACE_OUTER_BOUND ( 'NONE', #3173, .T. ) ;
#5388 = CARTESIAN_POINT ( 'NONE',  ( -74.24999999999980105, 15.00000000000014211, 10.00000000000017586 ) ) ;
#5389 = DIRECTION ( 'NONE',  ( 0.000000000000000000, 5.322451846059955323E-30, -1.000000000000000000 ) ) ;
#5390 = CARTESIAN_POINT ( 'NONE',  ( -3.319543390095988755, 7.321065037175355172, -0.01688885742771796192 ) ) ;
#5391 = ADVANCED_FACE ( 'NONE', ( #1777 ), #4516, .T. ) ;
#5392 =( LENGTH_UNIT ( ) NAMED_UNIT ( * ) SI_UNIT ( .MILLI., .METRE. ) );
#5393 = ORIENTED_EDGE ( 'NONE', *, *, #6246, .T. ) ;
#5394 = SURFACE_SIDE_STYLE ('',( #4084 ) ) ;
#5395 = CARTESIAN_POINT ( 'NONE',  ( 8.000000000000117240, 4.618802153517009401, -0.7145311798163467287 ) ) ;
#5396 = ADVANCED_FACE ( 'NONE', ( #5125 ), #1874, .T. ) ;
#5397 = DIRECTION ( 'NONE',  ( -1.000000000000000000, -8.881784197001244435E-16, 0.000000000000000000 ) ) ;
#5398 = CARTESIAN_POINT ( 'NONE',  ( 0.000000000000000000, -9.237604307034018802, -7.685468820183672278 ) ) ;
#5399 = AXIS2_PLACEMENT_3D ( 'NONE', #7216, #7342, #6559 ) ;
#5400 = CIRCLE ( 'NONE', #6056, 5.749999999999991118 ) ;
#5401 = DIRECTION ( 'NONE',  ( -1.000000000000000000, 0.000000000000000000, 0.000000000000000000 ) ) ;
#5402 = ORIENTED_EDGE ( 'NONE', *, *, #4961, .T. ) ;
#5403 = EDGE_LOOP ( 'NONE', ( #5150, #7666 ) ) ;
#5404 = CARTESIAN_POINT ( 'NONE',  ( 2.220446049250313081E-13, 9.237604307034075646, -0.7145311798163467287 ) ) ;
#5405 = VERTEX_POINT ( 'NONE', #400 ) ;
#5406 = DIRECTION ( 'NONE',  ( 1.000000000000000000, 0.000000000000000000, 0.000000000000000000 ) ) ;
#5407 = CYLINDRICAL_SURFACE ( 'NONE', #5694, 4.000000000000030198 ) ;
#5408 = EDGE_CURVE ( 'NONE', #7606, #79, #3048, .T. ) ;
#5409 = DIRECTION ( 'NONE',  ( -0.000000000000000000, -0.000000000000000000, 1.000000000000000000 ) ) ;
#5410 = CARTESIAN_POINT ( 'NONE',  ( 3.660532965668853667, -7.124194613927719466, -5.559246639419425248E-14 ) ) ;
#5411 = VERTEX_POINT ( 'NONE', #5048 ) ;
#5412 = CARTESIAN_POINT ( 'NONE',  ( 0.000000000000000000, 0.000000000000000000, 0.000000000000000000 ) ) ;
#5413 = ORIENTED_EDGE ( 'NONE', *, *, #3420, .T. ) ;
#5414 = DIRECTION ( 'NONE',  ( 0.000000000000000000, 1.224646799147300206E-16, 1.000000000000000000 ) ) ;
#5415 = FACE_OUTER_BOUND ( 'NONE', #8304, .T. ) ;
#5416 = ADVANCED_FACE ( 'NONE', ( #7707 ), #205, .T. ) ;
#5417 = VERTEX_POINT ( 'NONE', #1120 ) ;
#5418 = AXIS2_PLACEMENT_3D ( 'NONE', #3477, #3569, #2296 ) ;
#5419 = CARTESIAN_POINT ( 'NONE',  ( 4.000000000000003553, 9.714451465470119729E-14, 0.000000000000000000 ) ) ;
#5420 = AXIS2_PLACEMENT_3D ( 'NONE', #7518, #2241, #1542 ) ;
#5421 =( NAMED_UNIT ( * ) PLANE_ANGLE_UNIT ( ) SI_UNIT ( $, .RADIAN. ) );
#5422 = ORIENTED_EDGE ( 'NONE', *, *, #8604, .F. ) ;
#5423 = AXIS2_PLACEMENT_3D ( 'NONE', #1338, #1857, #728 ) ;
#5424 = CARTESIAN_POINT ( 'NONE',  ( -17.49999999999955236, 120.0000000000003268, 9.999999999999980460 ) ) ;
#5425 = ORIENTED_EDGE ( 'NONE', *, *, #27, .F. ) ;
#5426 = DIRECTION ( 'NONE',  ( 1.000000000000000000, 0.000000000000000000, 0.000000000000000000 ) ) ;
#5427 = AXIS2_PLACEMENT_3D ( 'NONE', #6827, #237, #4200 ) ;
#5428 = EDGE_CURVE ( 'NONE', #6245, #5503, #4954, .T. ) ;
#5429 = CLOSED_SHELL ( 'NONE', ( #3670, #6234, #1896, #362, #1637, #3826, #6365, #1657, #7398, #4186, #907, #2246, #2993, #2764, #62, #5416, #1446, #3530, #6927, #1713, #5917, #8240 ) ) ;
#5430 = DIRECTION ( 'NONE',  ( 0.000000000000000000, 1.000000000000000000, 1.795949010423047620E-16 ) ) ;
#5432 = EDGE_LOOP ( 'NONE', ( #2388, #1436, #1369, #4307 ) ) ;
#5431 = AXIS2_PLACEMENT_3D ( 'NONE', #2473, #3087, #3865 ) ;
#5433 = CARTESIAN_POINT ( 'NONE',  ( 50.00000000000004263, 500.0000000000000000, 50.00000000000000000 ) ) ;
#5434 = PRODUCT_DEFINITION_SHAPE ( 'NONE', 'NONE',  #8623 ) ;
#5435 = VECTOR ( 'NONE', #5064, 1000.000000000000000 ) ;
#5436 = FACE_OUTER_BOUND ( 'NONE', #4038, .T. ) ;
#5437 = CARTESIAN_POINT ( 'NONE',  ( -4.000000000000114575, -6.928203230275487456, -8.400000000000018119 ) ) ;
#5438 = FACE_OUTER_BOUND ( 'NONE', #3350, .T. ) ;
#5439 = VERTEX_POINT ( 'NONE', #3780 ) ;
#5440 = CIRCLE ( 'NONE', #1660, 10.49999999999999645 ) ;
#5441 = CARTESIAN_POINT ( 'NONE',  ( 0.000000000000000000, 0.000000000000000000, 18.00000000000000355 ) ) ;
#5442 = SURFACE_SIDE_STYLE ('',( #1431 ) ) ;
#5443 = VECTOR ( 'NONE', #252, 1000.000000000000000 ) ;
#5444 = EDGE_CURVE ( 'NONE', #579, #21, #3739, .T. ) ;
#5445 = CARTESIAN_POINT ( 'NONE',  ( 0.000000000000000000, 0.000000000000000000, 0.000000000000000000 ) ) ;
#5446=STYLED_ITEM('',(#8677),#2946);
#5447 = PRODUCT_DEFINITION_SHAPE ( 'NONE', 'NONE',  #8611 ) ;
#5448 = CARTESIAN_POINT ( 'NONE',  ( -7.999999999999894307, 3.115336682266945711, -8.080606868608583682 ) ) ;
#5449=STYLED_ITEM('',(#8670),#56);
#5450 = CARTESIAN_POINT ( 'NONE',  ( 1.310872448938211532, -8.480771745766629621, -8.082649155111216288 ) ) ;
#5451 = CARTESIAN_POINT ( 'NONE',  ( -3.660532965669703209, 7.124194613927820718, -8.399999999999687716 ) ) ;
#5452 = CARTESIAN_POINT ( 'NONE',  ( -7.999999999999890754, -0.7805016046292094778, 5.627856308147021051E-14 ) ) ;
#5453 = ORIENTED_EDGE ( 'NONE', *, *, #5686, .F. ) ;
#5454 = CARTESIAN_POINT ( 'NONE',  ( -3.999999999999781508, -6.928203230275875590, 0.000000000000000000 ) ) ;
#5455 = CARTESIAN_POINT ( 'NONE',  ( 6.123233995736776340E-15, 50.00000000000008527, 130.0000000000000000 ) ) ;
#5456 = CARTESIAN_POINT ( 'NONE',  ( -31.74999999999994316, 0.000000000000000000, 0.000000000000000000 ) ) ;
#5457 = DIRECTION ( 'NONE',  ( -1.000000000000000000, -1.421085471520200372E-14, 0.000000000000000000 ) ) ;
#5458 = ORIENTED_EDGE ( 'NONE', *, *, #7040, .F. ) ;
#5459 = ORIENTED_EDGE ( 'NONE', *, *, #7240, .F. ) ;
#5460 = SURFACE_STYLE_FILL_AREA ( #6167 ) ;
#5461 = FACE_OUTER_BOUND ( 'NONE', #4719, .T. ) ;
#5462 = AXIS2_PLACEMENT_3D ( 'NONE', #3485, #5497, #3445 ) ;
#5463 = CARTESIAN_POINT ( 'NONE',  ( -74.24999999999981526, 15.00000000000014211, 10.00000000000017586 ) ) ;
#5464 = VERTEX_POINT ( 'NONE', #1002 ) ;
#5465 = CIRCLE ( 'NONE', #2682, 8.000000000000007105 ) ;
#5466 = CARTESIAN_POINT ( 'NONE',  ( 0.000000000000000000, 60.00000000000000000, -45.00000000000000711 ) ) ;
#5467 = CARTESIAN_POINT ( 'NONE',  ( 334.9999999999997726, -20.00000000000062172, 49.99999999999999289 ) ) ;
#5468 = ORIENTED_EDGE ( 'NONE', *, *, #2831, .F. ) ;
#5469 = EDGE_CURVE ( 'NONE', #5857, #7532, #6323, .T. ) ;
#5470 = CIRCLE ( 'NONE', #1690, 24.50000000000000000 ) ;
#5471 = VERTEX_POINT ( 'NONE', #6437 ) ;
#5472 = CYLINDRICAL_SURFACE ( 'NONE', #5907, 14.99999999999986677 ) ;
#5473 = CARTESIAN_POINT ( 'NONE',  ( 0.000000000000000000, 0.000000000000000000, -8.400999999999992696 ) ) ;
#5474 = DIRECTION ( 'NONE',  ( 0.7071067811865456854, 8.659560562354910671E-17, -0.7071067811865493491 ) ) ;
#5475 = ORIENTED_EDGE ( 'NONE', *, *, #6627, .T. ) ;
#5476 = AXIS2_PLACEMENT_3D ( 'NONE', #7108, #7192, #1134 ) ;
#5477 = AXIS2_PLACEMENT_3D ( 'NONE', #5840, #4300, #2506 ) ;
#5478 = CARTESIAN_POINT ( 'NONE',  ( -34.99999999999966604, 120.0000000000003695, 9.999999999999980460 ) ) ;
#5479 = CARTESIAN_POINT ( 'NONE',  ( 8.000000000000119016, -1.555946510856292209, -0.06708870216344244020 ) ) ;
#5480 = ORIENTED_EDGE ( 'NONE', *, *, #5789, .T. ) ;
#5481 = AXIS2_PLACEMENT_3D ( 'NONE', #7369, #1412, #2159 ) ;
#5482 = EDGE_CURVE ( 'NONE', #4082, #2069, #475, .T. ) ;
#5483 = APPLICATION_CONTEXT ( 'automotive_design' ) ;
#5484 = DIRECTION ( 'NONE',  ( 0.000000000000000000, 0.000000000000000000, -1.000000000000000000 ) ) ;
#5485 = VECTOR ( 'NONE', #3580, 1000.000000000000000 ) ;
#5486 = CARTESIAN_POINT ( 'NONE',  ( -28.24999999999996447, 3.989921841591239357E-15, 18.00000000000000355 ) ) ;
#5487 = VECTOR ( 'NONE', #7411, 1000.000000000000000 ) ;
#5488 = CARTESIAN_POINT ( 'NONE',  ( 8.000000000000122569, -1.555946510856290210, -8.332911297836574249 ) ) ;
#5489 = CIRCLE ( 'NONE', #4226, 5.499999999999999112 ) ;
#5490 = CARTESIAN_POINT ( 'NONE',  ( 4.000000000000058620, 3.518949890710762585, 2.220446049250313081E-13 ) ) ;
#5491 = EDGE_CURVE ( 'NONE', #3875, #7175, #4511, .T. ) ;
#5492 = DIRECTION ( 'NONE',  ( 0.000000000000000000, 0.000000000000000000, 1.000000000000000000 ) ) ;
#5493 = EDGE_CURVE ( 'NONE', #1514, #6221, #7862, .T. ) ;
#5494 = DIRECTION ( 'NONE',  ( -1.000000000000000000, -8.881784197001244435E-16, -0.000000000000000000 ) ) ;
#5495 = ORIENTED_EDGE ( 'NONE', *, *, #4362, .F. ) ;
#5496 = AXIS2_PLACEMENT_3D ( 'NONE', #4111, #4280, #2847 ) ;
#5497 = DIRECTION ( 'NONE',  ( 4.622231866529366047E-33, -1.224646799147353454E-16, 1.000000000000000000 ) ) ;
#5498 = LINE ( 'NONE', #8147, #137 ) ;
#5499 = CARTESIAN_POINT ( 'NONE',  ( -1.954730054507676012E-32, 40.00000000000000711, 3.039269428540889921E-16 ) ) ;
#5500 = DIRECTION ( 'NONE',  ( -0.000000000000000000, -1.000000000000000000, -0.000000000000000000 ) ) ;
#5501 = EDGE_LOOP ( 'NONE', ( #1535, #2152 ) ) ;
#5502 = CARTESIAN_POINT ( 'NONE',  ( 4.000000000000058620, 3.518949890710762585, 2.220446049250313081E-13 ) ) ;
#5503 = VERTEX_POINT ( 'NONE', #3284 ) ;
#5504 = CARTESIAN_POINT ( 'NONE',  ( -7.999999999999890754, -3.867591403079264190, -7.902324684675469335 ) ) ;
#5505 = ORIENTED_EDGE ( 'NONE', *, *, #1912, .F. ) ;
#5506 = SHAPE_REPRESENTATION ( 'Servo motor', ( #7563 ), #6881 ) ;
#5507 = EDGE_CURVE ( 'NONE', #2978, #21, #3335, .T. ) ;
#5508 =( NAMED_UNIT ( * ) SI_UNIT ( $, .STERADIAN. ) SOLID_ANGLE_UNIT ( ) );
#5509 = PRODUCT_DEFINITION_SHAPE ( 'NONE', 'NONE',  #8620 ) ;
#5510 = DIRECTION ( 'NONE',  ( 1.000000000000000000, -1.774937036747276562E-30, 0.000000000000000000 ) ) ;
#5511 = ADVANCED_FACE ( 'NONE', ( #6649 ), #2689, .T. ) ;
#5512 = ORIENTED_EDGE ( 'NONE', *, *, #7464, .F. ) ;
#5513 = LINE ( 'NONE', #8075, #1801 ) ;
#5514 = CARTESIAN_POINT ( 'NONE',  ( -8.000000000000007105, -4.618802153517065356, -0.7145311798163467287 ) ) ;
#5515 = CARTESIAN_POINT ( 'NONE',  ( 350.0000000000000000, 59.99999999999992184, -60.70000000000002416 ) ) ;
#5516 = ORIENTED_EDGE ( 'NONE', *, *, #8274, .F. ) ;
#5517 = DIRECTION ( 'NONE',  ( -1.885870601543981347E-30, 1.000000000000000000, -7.405124331421681105E-16 ) ) ;
#5518 = EDGE_LOOP ( 'NONE', ( #6983, #5601, #4590, #3337 ) ) ;
#5519 = DIRECTION ( 'NONE',  ( 0.000000000000000000, -1.042965139114318115E-29, 1.000000000000000000 ) ) ;
#5520 = EDGE_CURVE ( 'NONE', #5835, #5464, #7339, .T. ) ;
#5521 = CARTESIAN_POINT ( 'NONE',  ( -7.999999999999785061, -4.618802153517121312, -8.400000000000018119 ) ) ;
#5522 = ORIENTED_EDGE ( 'NONE', *, *, #4213, .F. ) ;
#5523 = VECTOR ( 'NONE', #8391, 1000.000000000000114 ) ;
#5524 =( REPRESENTATION_RELATIONSHIP ('NONE','NONE', #1279, #6969 ) REPRESENTATION_RELATIONSHIP_WITH_TRANSFORMATION ( #5309 )SHAPE_REPRESENTATION_RELATIONSHIP( ) );
#5525 = CARTESIAN_POINT ( 'NONE',  ( 5.510910596163089556E-15, -40.00000000000000711, -3.039269428540889921E-16 ) ) ;
#5526 = FACE_OUTER_BOUND ( 'NONE', #8299, .T. ) ;
#5527 = ORIENTED_EDGE ( 'NONE', *, *, #8507, .F. ) ;
#5528 = DIRECTION ( 'NONE',  ( 0.000000000000000000, -0.5000000000000009992, -0.8660254037844380415 ) ) ;
#5529 = CARTESIAN_POINT ( 'NONE',  ( -8.000000000000007105, -4.618802153517065356, -7.685468820183672278 ) ) ;
#5530 = B_SPLINE_CURVE_WITH_KNOTS ( 'NONE', 3,
 ( #156, #6837, #2177, #7486, #6194, #202, #8176, #3567 ),
 .UNSPECIFIED., .F., .F.,
 ( 4, 2, 2, 4 ),
 ( 0.004673709593152776745, 0.005837709341828072745, 0.007001709090503368746, 0.009329708587853959012 ),
 .UNSPECIFIED. ) ;
#5531 = LINE ( 'NONE', #4788, #2306 ) ;
#5532 = ADVANCED_FACE ( 'NONE', ( #6014, #8598, #3943, #6605, #4, #3164, #5845, #8472 ), #2512, .F. ) ;
#5533 = DIRECTION ( 'NONE',  ( 0.000000000000000000, -0.000000000000000000, 1.000000000000000000 ) ) ;
#5534 = CARTESIAN_POINT ( 'NONE',  ( -4.339467034331054407, -6.732211846623885165, -8.399999999999826272 ) ) ;
#5535 = CARTESIAN_POINT ( 'NONE',  ( 7.999999999999563016, -4.618802153517398423, -0.7145311798163467287 ) ) ;
#5536 = ORIENTED_EDGE ( 'NONE', *, *, #1661, .F. ) ;
#5537 = CIRCLE ( 'NONE', #659, 5.749999999999991118 ) ;
#5538 = FACE_OUTER_BOUND ( 'NONE', #7016, .T. ) ;
#5539 = ORIENTED_EDGE ( 'NONE', *, *, #3193, .F. ) ;
#5540 = CARTESIAN_POINT ( 'NONE',  ( 5.000000000000115463, -14.99999999999990230, -20.00000000000001776 ) ) ;
#5541 = PLANE ( 'NONE',  #3241 ) ;
#5542 = ADVANCED_FACE ( 'NONE', ( #5300 ), #7212, .F. ) ;
#5543 = CYLINDRICAL_SURFACE ( 'NONE', #812, 4.250000000000003553 ) ;
#5544 = ORIENTED_EDGE ( 'NONE', *, *, #2789, .F. ) ;
#5545 = ORIENTED_EDGE ( 'NONE', *, *, #7943, .F. ) ;
#5546 = VECTOR ( 'NONE', #352, 1000.000000000000000 ) ;
#5547 = DIRECTION ( 'NONE',  ( 1.000000000000000000, 0.000000000000000000, 0.000000000000000000 ) ) ;
#5548 =( NAMED_UNIT ( * ) PLANE_ANGLE_UNIT ( ) SI_UNIT ( $, .RADIAN. ) );
#5549 = EDGE_CURVE ( 'NONE', #5371, #3622, #1736, .T. ) ;
#5550 = DIRECTION ( 'NONE',  ( -0.9237280213470678847, -0.3830490080632384942, 0.000000000000000000 ) ) ;
#5551 = ORIENTED_EDGE ( 'NONE', *, *, #455, .F. ) ;
#5552 = DIRECTION ( 'NONE',  ( -1.000000000000000000, 3.549874073494553124E-30, 0.000000000000000000 ) ) ;
#5553 = AXIS2_PLACEMENT_3D ( 'NONE', #1087, #4400, #5901 ) ;
#5554 = DIRECTION ( 'NONE',  ( 0.9237280213470682178, 0.3830490080632377725, 0.000000000000000000 ) ) ;
#5555 = VERTEX_POINT ( 'NONE', #148 ) ;
#5556 = DIRECTION ( 'NONE',  ( 0.000000000000000000, -5.908893405598423146E-30, 1.000000000000000000 ) ) ;
#5557 = EDGE_CURVE ( 'NONE', #3789, #2467, #1426, .T. ) ;
#5558 = ORIENTED_EDGE ( 'NONE', *, *, #6968, .T. ) ;
#5559 = FACE_BOUND ( 'NONE', #2989, .T. ) ;
#5560 = AXIS2_PLACEMENT_3D ( 'NONE', #3673, #5055, #1741 ) ;
#5561 = CARTESIAN_POINT ( 'NONE',  ( -4.681481898397175989, 6.534749472788146107, -5.458788531875063334E-14 ) ) ;
#5562 = AXIS2_PLACEMENT_3D ( 'NONE', #5844, #1851, #7087 ) ;
#5563 = ORIENTED_EDGE ( 'NONE', *, *, #3681, .T. ) ;
#5564 = ADVANCED_FACE ( 'NONE', ( #238, #5526 ), #4900, .F. ) ;
#5565 = CARTESIAN_POINT ( 'NONE',  ( 4.250000000000008882, 32.50000000000005684, 18.00000000000000355 ) ) ;
#5566 = CARTESIAN_POINT ( 'NONE',  ( -0.6543471694412733575, -8.859816792613717240, -7.903584543331185763 ) ) ;
#5567 = AXIS2_PLACEMENT_3D ( 'NONE', #3253, #1902, #5937 ) ;
#5568 = SHAPE_REPRESENTATION_RELATIONSHIP ( 'NONE' , 'NONE' ,  #6122, #3144 ) ;
#5569 = ORIENTED_EDGE ( 'NONE', *, *, #3834, .T. ) ;
#5570 = CARTESIAN_POINT ( 'NONE',  ( -3.999999999999892530, 6.928203230275431501, 0.000000000000000000 ) ) ;
#5571 = EDGE_CURVE ( 'NONE', #4545, #3409, #1525, .T. ) ;
#5572 = ORIENTED_EDGE ( 'NONE', *, *, #2058, .F. ) ;
#5573 = CARTESIAN_POINT ( 'NONE',  ( -79.99999999999980105, 15.00000000000012434, 10.00000000000017586 ) ) ;
#5574 = EDGE_CURVE ( 'NONE', #4545, #2313, #5233, .T. ) ;
#5575 = CLOSED_SHELL ( 'NONE', ( #7913, #7326, #4247, #1301, #6560, #8390, #6703, #882, #8414, #3128, #4910, #4680, #6413, #7034, #3945, #1410, #7667, #4462, #1371, #2029, #5004, #824, #4515, #3641, #3080, #6127, #3107 ) ) ;
#5576 = VECTOR ( 'NONE', #317, 1000.000000000000000 ) ;
#5577 = LINE ( 'NONE', #8097, #3234 ) ;
#5578 = LINE ( 'NONE', #5628, #4256 ) ;
#5579 = DIRECTION ( 'NONE',  ( -1.000000000000000000, -8.881784197001244435E-16, 0.000000000000000000 ) ) ;
#5580 = CIRCLE ( 'NONE', #1527, 4.499999999999990230 ) ;
#5581 = PRESENTATION_LAYER_ASSIGNMENT (  '', '', ( #845 ) ) ;
#5582 = CARTESIAN_POINT ( 'NONE',  ( 4.000000000000003553, -6.928203230275542523, -8.400000000000018119 ) ) ;
#5583 = CARTESIAN_POINT ( 'NONE',  ( 8.000000000000012434, -1.555946510856606624, -0.06708870216341396298 ) ) ;
#5584 = EDGE_LOOP ( 'NONE', ( #8400, #4594, #5925, #216 ) ) ;
#5585 = CIRCLE ( 'NONE', #4172, 0.4000000000000001887 ) ;
#5586 = PRODUCT_DEFINITION_SHAPE ( 'NONE', 'NONE',  #8625 ) ;
#5587 = DIRECTION ( 'NONE',  ( 3.851859888774471706E-33, 1.232595164407830946E-32, 1.000000000000000000 ) ) ;
#5588 = EDGE_LOOP ( 'NONE', ( #7874, #2961, #5505, #6711, #6665, #8207 ) ) ;
#5589 = B_SPLINE_CURVE_WITH_KNOTS ( 'NONE', 3,
 ( #3010, #5091, #5270, #7886, #1877, #1217 ),
 .UNSPECIFIED., .F., .F.,
 ( 4, 2, 4 ),
 ( 0.008240550023493446036, 0.01057684187039402771, 0.01291313371729461111 ),
 .UNSPECIFIED. ) ;
#5590 = EDGE_CURVE ( 'NONE', #6269, #3910, #2044, .T. ) ;
#5591 = PRODUCT_DEFINITION ( 'UNKNOWN', '', #350, #2547 ) ;
#5592 = DIRECTION ( 'NONE',  ( 0.000000000000000000, -5.322451846059954622E-30, 1.000000000000000000 ) ) ;
#5593 = ORIENTED_EDGE ( 'NONE', *, *, #6140, .F. ) ;
#5594 = CARTESIAN_POINT ( 'NONE',  ( -5.500000000000000000, 6.735557395310442023E-16, -50.00000000000000000 ) ) ;
#5595 = ORIENTED_EDGE ( 'NONE', *, *, #7335, .F. ) ;
#5596 = EDGE_LOOP ( 'NONE', ( #4367, #8542, #7759, #2188 ) ) ;
#5597 = PRESENTATION_LAYER_ASSIGNMENT (  '', '', ( #5449 ) ) ;
#5598 = EDGE_CURVE ( 'NONE', #3126, #2290, #5382, .T. ) ;
#5599 = CARTESIAN_POINT ( 'NONE',  ( -50.00000000000004263, -425.0000000000000000, 3.469446951953614189E-15 ) ) ;
#5600 = DIRECTION ( 'NONE',  ( 1.463706757734299248E-32, -1.000000000000000000, -5.238529448733281520E-32 ) ) ;
#5601 = ORIENTED_EDGE ( 'NONE', *, *, #4235, .T. ) ;
#5602 = DIRECTION ( 'NONE',  ( 0.000000000000000000, -0.000000000000000000, 1.000000000000000000 ) ) ;
#5603 = CARTESIAN_POINT ( 'NONE',  ( -8.000000000000005329, 3.115336682266933277, -8.080606868608525062 ) ) ;
#5604 = CARTESIAN_POINT ( 'NONE',  ( -350.0000000000001705, 59.99999999999998579, 70.00000000000000000 ) ) ;
#5605 = EDGE_LOOP ( 'NONE', ( #2812, #5361, #794 ) ) ;
#5606 = FACE_OUTER_BOUND ( 'NONE', #766, .T. ) ;
#5607 = EDGE_CURVE ( 'NONE', #1223, #6543, #3494, .T. ) ;
#5608 = ORIENTED_EDGE ( 'NONE', *, *, #153, .T. ) ;
#5609 = CARTESIAN_POINT ( 'NONE',  ( 8.000000000000014211, -5.497230663963304033E-14, 4.400000000000696687 ) ) ;
#5610 = B_SPLINE_CURVE_WITH_KNOTS ( 'NONE', 3,
 ( #4461, #7648, #6430, #4422, #4945, #3157 ),
 .UNSPECIFIED., .F., .F.,
 ( 4, 2, 4 ),
 ( 2.380731629389045982E-07, 0.002336973833157555535, 0.004673709593152172194 ),
 .UNSPECIFIED. ) ;
#5611 = B_SPLINE_CURVE_WITH_KNOTS ( 'NONE', 3,
 ( #6782, #1417, #4069, #8591, #806, #6007 ),
 .UNSPECIFIED., .F., .F.,
 ( 4, 2, 4 ),
 ( 0.008240550023493515425, 0.01057684187039419250, 0.01291313371729486958 ),
 .UNSPECIFIED. ) ;
#5612 = DIRECTION ( 'NONE',  ( -0.000000000000000000, -0.000000000000000000, 1.000000000000000000 ) ) ;
#5613 = ORIENTED_EDGE ( 'NONE', *, *, #5836, .T. ) ;
#5614 = CIRCLE ( 'NONE', #4898, 8.000000000000001776 ) ;
#5615 = CARTESIAN_POINT ( 'NONE',  ( 8.400000000000018119, -5.551115123125777653E-14, -4.399999999999364420 ) ) ;
#5616 = ADVANCED_FACE ( 'NONE', ( #8172 ), #4160, .T. ) ;
#5617 = AXIS2_PLACEMENT_3D ( 'NONE', #4708, #2047, #3261 ) ;
#5618 =( NAMED_UNIT ( * ) PLANE_ANGLE_UNIT ( ) SI_UNIT ( $, .RADIAN. ) );
#5619 = ORIENTED_EDGE ( 'NONE', *, *, #6180, .T. ) ;
#5620 = EDGE_CURVE ( 'NONE', #3622, #2009, #5045, .T. ) ;
#5621 = DIRECTION ( 'NONE',  ( -0.000000000000000000, -1.000000000000000000, -0.000000000000000000 ) ) ;
#5622 = AXIS2_PLACEMENT_3D ( 'NONE', #6960, #4296, #8305 ) ;
#5623 = EDGE_LOOP ( 'NONE', ( #1602, #7323 ) ) ;
#5624 = DIRECTION ( 'NONE',  ( -3.919652622816902408E-30, -3.944304526105059027E-30, 1.000000000000000000 ) ) ;
#5625 = AXIS2_PLACEMENT_3D ( 'NONE', #1484, #4100, #4008 ) ;
#5626 = CARTESIAN_POINT ( 'NONE',  ( 4.681481898397195529, -6.534749472788381475, -8.399999999999842260 ) ) ;
#5627 = VECTOR ( 'NONE', #2416, 1000.000000000000000 ) ;
#5628 = CARTESIAN_POINT ( 'NONE',  ( -34.92499999999998295, 0.000000000000000000, 5.559999999999998721 ) ) ;
#5629 = AXIS2_PLACEMENT_3D ( 'NONE', #3018, #276, #5748 ) ;
#5630 = ADVANCED_FACE ( 'NONE', ( #2128 ), #4781, .T. ) ;
#5631 = DIRECTION ( 'NONE',  ( 0.000000000000000000, 0.000000000000000000, 1.000000000000000000 ) ) ;
#5632 = CARTESIAN_POINT ( 'NONE',  ( -4.680456609903821175, -6.535341423376089587, -8.383111142572069241 ) ) ;
#5633 = CARTESIAN_POINT ( 'NONE',  ( 32.49999999999997158, 1.387778780781445676E-14, 18.00000000000000355 ) ) ;
#5634 = ORIENTED_EDGE ( 'NONE', *, *, #245, .F. ) ;
#5635 = CARTESIAN_POINT ( 'NONE',  ( -50.00000000000004263, 500.0000000000000000, -50.00000000000000000 ) ) ;
#5636 = EDGE_LOOP ( 'NONE', ( #1521, #6640, #198 ) ) ;
#5637 = PRESENTATION_STYLE_ASSIGNMENT (( #1017 ) ) ;
#5638 = AXIS2_PLACEMENT_3D ( 'NONE', #2983, #323, #490 ) ;
#5639 = CIRCLE ( 'NONE', #2842, 4.000000000000030198 ) ;
#5640 = DIRECTION ( 'NONE',  ( 1.000000000000000000, 2.715219353702835081E-15, 0.000000000000000000 ) ) ;
#5641 = ORIENTED_EDGE ( 'NONE', *, *, #5105, .T. ) ;
#5642 = AXIS2_PLACEMENT_3D ( 'NONE', #7622, #2220, #6933 ) ;
#5643 = EDGE_CURVE ( 'NONE', #3935, #3744, #54, .T. ) ;
#5644 = LINE ( 'NONE', #2917, #6384 ) ;
#5645 = ORIENTED_EDGE ( 'NONE', *, *, #2704, .T. ) ;
#5646 = ORIENTED_EDGE ( 'NONE', *, *, #2840, .F. ) ;
#5647 = AXIS2_PLACEMENT_3D ( 'NONE', #4813, #7470, #1494 ) ;
#5648 = DIRECTION ( 'NONE',  ( -1.000000000000000000, -8.881784197001244435E-16, -0.000000000000000000 ) ) ;
#5649 = VERTEX_POINT ( 'NONE', #5933 ) ;
#5650 = CARTESIAN_POINT ( 'NONE',  ( -2.300000000000024247, 6.809036203259282560E-16, -5.559999999999998721 ) ) ;
#5651 = LINE ( 'NONE', #7673, #5007 ) ;
#5652 = EDGE_CURVE ( 'NONE', #988, #7562, #4699, .T. ) ;
#5653 = EDGE_LOOP ( 'NONE', ( #8398, #4025, #7945, #5171 ) ) ;
#5654 = CARTESIAN_POINT ( 'NONE',  ( 0.000000000000000000, 0.000000000000000000, -8.400000000000018119 ) ) ;
#5655 = DIRECTION ( 'NONE',  ( 0.5000000000000029976, -0.8660254037844370423, 0.000000000000000000 ) ) ;
#5656 = DIRECTION ( 'NONE',  ( -1.058471975245258048E-16, 8.736544766236844851E-16, -1.000000000000000000 ) ) ;
#5657 = ORIENTED_EDGE ( 'NONE', *, *, #4717, .T. ) ;
#5658 = CARTESIAN_POINT ( 'NONE',  ( 10.00000000000000888, 0.000000000000000000, 4.440892098500626162E-13 ) ) ;
#5659 = VERTEX_POINT ( 'NONE', #8005 ) ;
#5660 = CARTESIAN_POINT ( 'NONE',  ( -7.999999999999785061, 4.618802153516870845, -7.685468820183672278 ) ) ;
#5661 = APPLICATION_CONTEXT ( 'automotive_design' ) ;
#5662 = DIRECTION ( 'NONE',  ( -0.9237280213470678847, -0.3830490080632384942, 0.000000000000000000 ) ) ;
#5663 = CARTESIAN_POINT ( 'NONE',  ( -15.00000000000000000, -1.111739529205948433E-31, 6.018531076210101093E-32 ) ) ;
#5664 = EDGE_CURVE ( 'NONE', #2338, #7258, #2648, .T. ) ;
#5665 = VERTEX_POINT ( 'NONE', #5974 ) ;
#5666 = DIRECTION ( 'NONE',  ( -1.000000000000000000, 1.774937036747276562E-30, 0.000000000000000000 ) ) ;
#5667 = AXIS2_PLACEMENT_3D ( 'NONE', #5813, #3171, #7096 ) ;
#5668 = ORIENTED_EDGE ( 'NONE', *, *, #4315, .T. ) ;
#5669 = ORIENTED_EDGE ( 'NONE', *, *, #4427, .T. ) ;
#5670 = CARTESIAN_POINT ( 'NONE',  ( 0.000000000000000000, -1.040834085586084257E-14, -120.0000000000000000 ) ) ;
#5671 = AXIS2_PLACEMENT_3D ( 'NONE', #2086, #3996, #5977 ) ;
#5672 = DIRECTION ( 'NONE',  ( -3.851859888774471706E-33, -1.232595164407830946E-32, -1.000000000000000000 ) ) ;
#5673 = DIRECTION ( 'NONE',  ( -1.000000000000000000, -8.881784197001244435E-16, 0.000000000000000000 ) ) ;
#5674 = ADVANCED_FACE ( 'NONE', ( #1905 ), #6657, .T. ) ;
#5675 = CARTESIAN_POINT ( 'NONE',  ( -44.99999999999992895, 425.0000000000000000, 25.00000000000001066 ) ) ;
#5676 = DIRECTION ( 'NONE',  ( -7.703719777548943412E-34, 0.000000000000000000, 1.000000000000000000 ) ) ;
#5677 = DIRECTION ( 'NONE',  ( 0.000000000000000000, 0.000000000000000000, 1.000000000000000000 ) ) ;
#5678 = ADVANCED_FACE ( 'NONE', ( #8480, #7825, #729 ), #3860, .T. ) ;
#5679 = FACE_OUTER_BOUND ( 'NONE', #3037, .T. ) ;
#5680 = ORIENTED_EDGE ( 'NONE', *, *, #1647, .F. ) ;
#5681 = EDGE_CURVE ( 'NONE', #8336, #3789, #793, .T. ) ;
#5682 = LINE ( 'NONE', #6326, #6971 ) ;
#5683 = ORIENTED_EDGE ( 'NONE', *, *, #4152, .F. ) ;
#5684 = MECHANICAL_DESIGN_GEOMETRIC_PRESENTATION_REPRESENTATION (  '', ( #5820 ), #4266 ) ;
#5685 = MANIFOLD_SOLID_BREP ( 'EndChamfer', #1111 ) ;
#5686 = EDGE_CURVE ( 'NONE', #5923, #7803, #6722, .T. ) ;
#5687 = DIRECTION ( 'NONE',  ( -1.463706757734299248E-32, 1.000000000000000000, 5.238529448733281520E-32 ) ) ;
#5688 = DIRECTION ( 'NONE',  ( -3.851859888774471706E-33, -1.232595164407830946E-32, -1.000000000000000000 ) ) ;
#5689 = VERTEX_POINT ( 'NONE', #644 ) ;
#5690 = AXIS2_PLACEMENT_3D ( 'NONE', #1403, #4139, #7456 ) ;
#5691 = ORIENTED_EDGE ( 'NONE', *, *, #7291, .F. ) ;
#5692 = DIRECTION ( 'NONE',  ( -3.851859888774471706E-33, 7.598173571352223877E-18, -1.000000000000000000 ) ) ;
#5693 = AXIS2_PLACEMENT_3D ( 'NONE', #4562, #3955, #5975 ) ;
#5694 = AXIS2_PLACEMENT_3D ( 'NONE', #5456, #7610, #834 ) ;
#5695 = CARTESIAN_POINT ( 'NONE',  ( 0.000000000000000000, -3.469446951953614189E-15, 128.9999999999999432 ) ) ;
#5696 = LINE ( 'NONE', #6099, #724 ) ;
#5697 = CARTESIAN_POINT ( 'NONE',  ( 0.000000000000000000, 0.000000000000000000, 0.000000000000000000 ) ) ;
#5698 = VERTEX_POINT ( 'NONE', #4863 ) ;
#5699 = DIRECTION ( 'NONE',  ( -7.703719777548943412E-34, 0.000000000000000000, 1.000000000000000000 ) ) ;
#5700 = CARTESIAN_POINT ( 'NONE',  ( 0.000000000000000000, 0.000000000000000000, 0.000000000000000000 ) ) ;
#5701 = SHAPE_DEFINITION_REPRESENTATION ( #3692, #1279 ) ;
#5702 = ORIENTED_EDGE ( 'NONE', *, *, #391, .T. ) ;
#5703 = CARTESIAN_POINT ( 'NONE',  ( 139.9999999999994316, 3.469446951953614189E-14, -1.443289932012703503E-12 ) ) ;
#5704 = DIRECTION ( 'NONE',  ( -1.000000000000000000, 0.000000000000000000, 0.000000000000000000 ) ) ;
#5705 = EDGE_CURVE ( 'NONE', #6198, #7037, #2310, .T. ) ;
#5706 = DIRECTION ( 'NONE',  ( -1.000000000000000000, -8.881784197001244435E-16, 0.000000000000000000 ) ) ;
#5707 = EDGE_LOOP ( 'NONE', ( #7227, #7864, #7551, #7540 ) ) ;
#5708 = LINE ( 'NONE', #7760, #427 ) ;
#5709 = DIRECTION ( 'NONE',  ( 0.000000000000000000, 0.000000000000000000, 1.000000000000000000 ) ) ;
#5710 =( LENGTH_UNIT ( ) NAMED_UNIT ( * ) SI_UNIT ( .MILLI., .METRE. ) );
#5711 = ORIENTED_EDGE ( 'NONE', *, *, #6427, .T. ) ;
#5712 = ORIENTED_EDGE ( 'NONE', *, *, #3454, .T. ) ;
#5713 = CARTESIAN_POINT ( 'NONE',  ( 3.999999999999559464, 6.928203230274987412, -8.400000000000018119 ) ) ;
#5714 = EDGE_LOOP ( 'NONE', ( #4314, #3479 ) ) ;
#5715 = DIRECTION ( 'NONE',  ( 0.000000000000000000, 0.000000000000000000, 1.000000000000000000 ) ) ;
#5716 = EDGE_CURVE ( 'NONE', #2801, #7042, #2343, .T. ) ;
#5717 = CIRCLE ( 'NONE', #1931, 8.000000000000007105 ) ;
#5718 = DIRECTION ( 'NONE',  ( -1.000000000000000000, -0.000000000000000000, -0.000000000000000000 ) ) ;
#5719 = CARTESIAN_POINT ( 'NONE',  ( -8.000000000000673239, 4.618802153517287401, -7.685468820183672278 ) ) ;
#5720 = DIRECTION ( 'NONE',  ( -1.000000000000000000, -8.881784197001244435E-16, 0.000000000000000000 ) ) ;
#5721 = FACE_OUTER_BOUND ( 'NONE', #6959, .T. ) ;
#5722 = CARTESIAN_POINT ( 'NONE',  ( 8.000000000000008882, 3.115336682267075386, -0.3193931313915240877 ) ) ;
#5723 = AXIS2_PLACEMENT_3D ( 'NONE', #5814, #1911, #6570 ) ;
#5724 = CYLINDRICAL_SURFACE ( 'NONE', #7285, 4.250000000000014211 ) ;
#5725 = ORIENTED_EDGE ( 'NONE', *, *, #7377, .F. ) ;
#5726 = PLANE ( 'NONE',  #6006 ) ;
#5727 = ORIENTED_EDGE ( 'NONE', *, *, #6479, .F. ) ;
#5728 = ADVANCED_FACE ( 'NONE', ( #3495 ), #3315, .T. ) ;
#5729 = ADVANCED_FACE ( 'NONE', ( #81 ), #3456, .T. ) ;
#5730 = MANIFOLD_SOLID_BREP ( 'Chamfer2', #4874 ) ;
#5731 = CIRCLE ( 'NONE', #3476, 8.000000000000007105 ) ;
#5732 = PRODUCT ( 'socket head cap screw_am_B18.3.1M - 10 x 1.5 x 130 Hex SHCS -- 32NHX', 'socket head cap screw_am_B18.3.1M - 10 x 1.5 x 130 Hex SHCS -- 32NHX', '', ( #2013 ) ) ;
#5733 = DIRECTION ( 'NONE',  ( 1.463706757734299248E-32, -1.000000000000000000, -5.238529448733281520E-32 ) ) ;
#5734 = CARTESIAN_POINT ( 'NONE',  ( -82.49999999999941735, 120.0000000000003268, -2.775557561562891351E-14 ) ) ;
#5735 = ORIENTED_EDGE ( 'NONE', *, *, #3765, .T. ) ;
#5736 = CARTESIAN_POINT ( 'NONE',  ( 5.000000000000004441, -2.342598717236951789, 4.057500000000047180 ) ) ;
#5737 = VECTOR ( 'NONE', #5552, 1000.000000000000000 ) ;
#5738 = EDGE_CURVE ( 'NONE', #758, #4193, #5585, .T. ) ;
#5739 = CONICAL_SURFACE ( 'NONE', #1955, 8.000000000000007105, 1.047197551196597631 ) ;
#5740 = PRODUCT_DEFINITION_SHAPE ( 'NONE', 'NONE',  #8628 ) ;
#5741 = CARTESIAN_POINT ( 'NONE',  ( -31.74999999999994316, -2.238274855355529073E-28, 5.000000000000034639 ) ) ;
#5742 = ORIENTED_EDGE ( 'NONE', *, *, #1124, .T. ) ;
#5743 = DIRECTION ( 'NONE',  ( 0.000000000000000000, 0.000000000000000000, -1.000000000000000000 ) ) ;
#5744 = ADVANCED_FACE ( 'NONE', ( #7543 ), #8195, .T. ) ;
#5745 = COLOUR_RGB ( '',0.7921568627450980005, 0.8196078431372548767, 0.9333333333333333481 ) ;
#5746 = CARTESIAN_POINT ( 'NONE',  ( -4.681481898396900654, 6.534749472788120350, -8.400000000000067857 ) ) ;
#5747 = PRODUCT_CONTEXT ( 'NONE', #5483, 'mechanical' ) ;
#5748 = DIRECTION ( 'NONE',  ( 0.000000000000000000, 1.224646799147288373E-16, 1.000000000000000000 ) ) ;
#5749 = FACE_OUTER_BOUND ( 'NONE', #8578, .T. ) ;
#5750 = ORIENTED_EDGE ( 'NONE', *, *, #1661, .T. ) ;
#5751 = CARTESIAN_POINT ( 'NONE',  ( -44.99999999999992895, -500.0000000000000000, 45.00000000000000711 ) ) ;
#5752 = EDGE_CURVE ( 'NONE', #2098, #4479, #5286, .T. ) ;
#5753 = MANIFOLD_SOLID_BREP ( 'Hex', #5575 ) ;
#5754 = ORIENTED_EDGE ( 'NONE', *, *, #6591, .T. ) ;
#5755 = CARTESIAN_POINT ( 'NONE',  ( -8.000000000000673239, 4.618802153517287401, -0.7145311798163467287 ) ) ;
#5756 = ORIENTED_EDGE ( 'NONE', *, *, #7511, .T. ) ;
#5757 = DIRECTION ( 'NONE',  ( 2.728201748236233471E-33, -0.7071067811865491270, 0.7071067811865459074 ) ) ;
#5758 = FACE_BOUND ( 'NONE', #7458, .T. ) ;
#5759 = CARTESIAN_POINT ( 'NONE',  ( -7.999999999999785061, 4.618802153516870845, -7.685468820183672278 ) ) ;
#5760 = DIRECTION ( 'NONE',  ( 0.000000000000000000, 0.000000000000000000, -1.000000000000000000 ) ) ;
#5761 = AXIS2_PLACEMENT_3D ( 'NONE', #6355, #8220, #7482 ) ;
#5762 = LINE ( 'NONE', #430, #7811 ) ;
#5763 = CARTESIAN_POINT ( 'NONE',  ( 1.110223024625156540E-13, -410.0000000000000568, -6.938893903907228378E-14 ) ) ;
#5764 = EDGE_CURVE ( 'NONE', #4696, #1999, #5498, .T. ) ;
#5765 = CARTESIAN_POINT ( 'NONE',  ( -3.999999999999892530, 6.928203230275431501, -8.400000000000018119 ) ) ;
#5766 = ORIENTED_EDGE ( 'NONE', *, *, #1328, .T. ) ;
#5767 = AXIS2_PLACEMENT_3D ( 'NONE', #1717, #6394, #423 ) ;
#5768 = FILL_AREA_STYLE_COLOUR ( '', #2111 ) ;
#5769 = VERTEX_POINT ( 'NONE', #3532 ) ;
#5770 = CARTESIAN_POINT ( 'NONE',  ( 8.000000000000007105, -4.618802153517121312, -0.7145311798163467287 ) ) ;
#5771 = CONTEXT_DEPENDENT_SHAPE_REPRESENTATION ( #3405, #6143 ) ;
#5772 = EDGE_CURVE ( 'NONE', #4565, #8027, #3579, .T. ) ;
#5773 = DIRECTION ( 'NONE',  ( 3.851859888774471706E-33, -7.598173571352216173E-18, 1.000000000000000000 ) ) ;
#5774 = EDGE_CURVE ( 'NONE', #698, #863, #2923, .T. ) ;
#5775 = CIRCLE ( 'NONE', #4221, 25.00000000000000711 ) ;
#5776 = VERTEX_POINT ( 'NONE', #1906 ) ;
#5777 = LINE ( 'NONE', #7104, #5071 ) ;
#5778 = AXIS2_PLACEMENT_3D ( 'NONE', #6852, #7502, #2057 ) ;
#5779 = APPLICATION_CONTEXT ( 'automotive_design' ) ;
#5780 = CONICAL_SURFACE ( 'NONE', #1707, 38.74999999999999289, 0.7853981633974447263 ) ;
#5781 = CARTESIAN_POINT ( 'NONE',  ( 5.499999999999999112, 60.00000000000000000, 50.00000000000000000 ) ) ;
#5782 = AXIS2_PLACEMENT_3D ( 'NONE', #1370, #3371, #4598 ) ;
#5783 = CARTESIAN_POINT ( 'NONE',  ( 8.000000000000007105, 4.618802153516899267, -0.7145311798163467287 ) ) ;
#5784 = CARTESIAN_POINT ( 'NONE',  ( -4.000000000000891731, 6.928203230275542523, 0.000000000000000000 ) ) ;
#5785 = EDGE_LOOP ( 'NONE', ( #3980, #7158, #2940, #2998 ) ) ;
#5786 = EDGE_CURVE ( 'NONE', #1855, #1989, #4950, .T. ) ;
#5787 = PLANE ( 'NONE',  #2822 ) ;
#5788 = CARTESIAN_POINT ( 'NONE',  ( 7.347286611337029427, 4.995646404165263732, -7.903039949738243308 ) ) ;
#5789 = EDGE_CURVE ( 'NONE', #3192, #4476, #565, .T. ) ;
#5790 = DIRECTION ( 'NONE',  ( -1.000000000000000000, 1.774937036747276562E-30, 0.000000000000000000 ) ) ;
#5791 = APPLICATION_PROTOCOL_DEFINITION ( 'draft international standard', 'automotive_design', 1998, #1030 ) ;
#5792 = CARTESIAN_POINT ( 'NONE',  ( 0.000000000000000000, 0.000000000000000000, -10.00000000000006395 ) ) ;
#5793 = EDGE_CURVE ( 'NONE', #5417, #1241, #1863, .T. ) ;
#5794 = LINE ( 'NONE', #4495, #2359 ) ;
#5795 = EDGE_LOOP ( 'NONE', ( #1011, #5370 ) ) ;
#5796 = ADVANCED_FACE ( 'NONE', ( #5354 ), #5739, .T. ) ;
#5797 = DIRECTION ( 'NONE',  ( -3.549874073494552424E-30, 0.5000000000000009992, 0.8660254037844380415 ) ) ;
#5798 = ORIENTED_EDGE ( 'NONE', *, *, #2377, .T. ) ;
#5799 = CARTESIAN_POINT ( 'NONE',  ( 6.123233995736764507E-15, 49.99999999999999289, -109.9999999999999574 ) ) ;
#5800 = PRODUCT ( 'flat washer narrow_am_B18.22M - Plain washer, 10 mm, narrow', 'flat washer narrow_am_B18.22M - Plain washer, 10 mm, narrow', '', ( #5097 ) ) ;
#5801 = ORIENTED_EDGE ( 'NONE', *, *, #5306, .T. ) ;
#5802 = CARTESIAN_POINT ( 'NONE',  ( -6.689127551061941013, -5.375634714785060275, -0.3173508448887821798 ) ) ;
#5803 = DIRECTION ( 'NONE',  ( -1.000000000000000000, 0.000000000000000000, 0.000000000000000000 ) ) ;
#5804 = CARTESIAN_POINT ( 'NONE',  ( -82.49999999999941735, 120.0000000000003268, -2.775557561562891351E-14 ) ) ;
#5805 = DIRECTION ( 'NONE',  ( 1.463706757734299248E-32, -1.000000000000000000, -5.238529448733281520E-32 ) ) ;
#5806 = DIRECTION ( 'NONE',  ( 0.000000000000000000, -1.064348848528640685E-29, 1.000000000000000000 ) ) ;
#5807 = CARTESIAN_POINT ( 'NONE',  ( -6.661338147750939243E-13, -9.237604307034462892, -8.400000000000018119 ) ) ;
#5808 = PLANE ( 'NONE',  #1711 ) ;
#5809 = VERTEX_POINT ( 'NONE', #2651 ) ;
#5810 = PRESENTATION_STYLE_ASSIGNMENT (( #5213 ) ) ;
#5811 = VERTEX_POINT ( 'NONE', #2085 ) ;
#5812 = EDGE_CURVE ( 'NONE', #5338, #8164, #1250, .T. ) ;
#5813 = CARTESIAN_POINT ( 'NONE',  ( 0.000000000000000000, -299.9999999999999432, -2.775557561562891351E-14 ) ) ;
#5814 = CARTESIAN_POINT ( 'NONE',  ( 0.000000000000000000, -294.9999999999998295, -2.775557561562891351E-14 ) ) ;
#5815 = ORIENTED_EDGE ( 'NONE', *, *, #3859, .F. ) ;
#5816 = AXIS2_PLACEMENT_3D ( 'NONE', #385, #3733, #3776 ) ;
#5817 = EDGE_LOOP ( 'NONE', ( #2868, #574, #6388, #6243, #4270, #2245 ) ) ;
#5818 = CARTESIAN_POINT ( 'NONE',  ( 0.000000000000000000, 0.000000000000000000, 0.000000000000000000 ) ) ;
#5819 = B_SPLINE_CURVE_WITH_KNOTS ( 'NONE', 3,
 ( #7973, #2006, #7276, #6578, #5318, #4622 ),
 .UNSPECIFIED., .F., .F.,
 ( 4, 2, 4 ),
 ( 0.01291313371729446019, 0.01525081363757301890, 0.01758849355785157761 ),
 .UNSPECIFIED. ) ;
#5820=STYLED_ITEM('',(#8670),#5685);
#5821 = EDGE_CURVE ( 'NONE', #5093, #6993, #4533, .T. ) ;
#5822 = CARTESIAN_POINT ( 'NONE',  ( 1.110223024625156540E-13, -410.0000000000000568, 24.49999999999992895 ) ) ;
#5823 = CARTESIAN_POINT ( 'NONE',  ( 0.000000000000000000, -3.469446951953614189E-15, 130.0000000000000000 ) ) ;
#5824 = CARTESIAN_POINT ( 'NONE',  ( 3.999999999999559464, 6.928203230274987412, 0.000000000000000000 ) ) ;
#5825 = VERTEX_POINT ( 'NONE', #1907 ) ;
#5826 = DIRECTION ( 'NONE',  ( -0.9237280213470678847, -0.3830490080632384942, 0.000000000000000000 ) ) ;
#5827 = LINE ( 'NONE', #3141, #1253 ) ;
#5828 = DIRECTION ( 'NONE',  ( 0.000000000000000000, 0.000000000000000000, 1.000000000000000000 ) ) ;
#5829 = EDGE_CURVE ( 'NONE', #6788, #1251, #6284, .T. ) ;
#5830 = DIRECTION ( 'NONE',  ( -1.000000000000000000, -3.083952846180992055E-15, 0.000000000000000000 ) ) ;
#5831 = ORIENTED_EDGE ( 'NONE', *, *, #8057, .T. ) ;
#5832 = B_SPLINE_CURVE_WITH_KNOTS ( 'NONE', 3,
 ( #5970, #2079, #8045, #3382, #4125, #2817 ),
 .UNSPECIFIED., .F., .F.,
 ( 4, 2, 4 ),
 ( 0.01291313371729460764, 0.01525081363757309350, 0.01758849355785158108 ),
 .UNSPECIFIED. ) ;
#5833 = LINE ( 'NONE', #667, #425 ) ;
#5834 = MANIFOLD_SOLID_BREP ( 'EndChamfer', #5429 ) ;
#5835 = VERTEX_POINT ( 'NONE', #1721 ) ;
#5836 = EDGE_CURVE ( 'NONE', #7888, #1663, #4878, .T. ) ;
#5837 = DIRECTION ( 'NONE',  ( 0.000000000000000000, -1.213383262747659708E-29, 1.000000000000000000 ) ) ;
#5838 = VERTEX_POINT ( 'NONE', #5675 ) ;
#5839 = CARTESIAN_POINT ( 'NONE',  ( -8.000000000000007105, -4.618802153517398423, -8.400000000000018119 ) ) ;
#5840 = CARTESIAN_POINT ( 'NONE',  ( 0.000000000000000000, 0.000000000000000000, 0.000000000000000000 ) ) ;
#5841 = DIRECTION ( 'NONE',  ( -7.420547859534711256E-34, 1.000000000000000000, 1.224646799147352961E-16 ) ) ;
#5842 = CARTESIAN_POINT ( 'NONE',  ( -8.000000000000007105, -4.618802153517065356, -7.685468820183672278 ) ) ;
#5843 = DIRECTION ( 'NONE',  ( -1.000000000000000000, 2.842664852890546338E-35, -7.703719777548943412E-34 ) ) ;
#5844 = CARTESIAN_POINT ( 'NONE',  ( 1.110223024625156540E-13, -410.0000000000000568, -6.938893903907228378E-14 ) ) ;
#5845 = FACE_BOUND ( 'NONE', #6264, .T. ) ;
#5846 = PLANE ( 'NONE',  #3102 ) ;
#5847 = VERTEX_POINT ( 'NONE', #3074 ) ;
#5848 = EDGE_CURVE ( 'NONE', #3300, #2978, #5876, .T. ) ;
#5849 = ORIENTED_EDGE ( 'NONE', *, *, #7810, .F. ) ;
#5850 = CARTESIAN_POINT ( 'NONE',  ( -50.00000000000004263, 425.0000000000000000, 3.469446951953614189E-15 ) ) ;
#5851 = CIRCLE ( 'NONE', #6944, 5.749999999999985789 ) ;
#5852 = CARTESIAN_POINT ( 'NONE',  ( 3.999999999999559464, 6.928203230274987412, 0.000000000000000000 ) ) ;
#5853 = CONTEXT_DEPENDENT_SHAPE_REPRESENTATION ( #4858, #5447 ) ;
#5854 = VERTEX_POINT ( 'NONE', #1764 ) ;
#5855 = CIRCLE ( 'NONE', #8191, 4.499999999999990230 ) ;
#5856 = CARTESIAN_POINT ( 'NONE',  ( 4.000000000000003553, -3.518949890710769690, 0.000000000000000000 ) ) ;
#5857 = VERTEX_POINT ( 'NONE', #3850 ) ;
#5858 = DIRECTION ( 'NONE',  ( -1.000000000000000000, 3.549874073494553124E-30, 0.000000000000000000 ) ) ;
#5859 = EDGE_CURVE ( 'NONE', #3472, #6699, #2370, .T. ) ;
#5860 = ORIENTED_EDGE ( 'NONE', *, *, #208, .T. ) ;
#5861 = CIRCLE ( 'NONE', #3325, 4.250000000000006217 ) ;
#5862 = CARTESIAN_POINT ( 'NONE',  ( -7.347286611337213280, -4.995646404165206889, -7.903039949738177583 ) ) ;
#5863 = DIRECTION ( 'NONE',  ( -1.000000000000000000, 1.774937036747276562E-30, 0.000000000000000000 ) ) ;
#5864 = MANIFOLD_SOLID_BREP ( 'Hex', #1654 ) ;
#5865 = CARTESIAN_POINT ( 'NONE',  ( 0.000000000000000000, 0.000000000000000000, 0.000000000000000000 ) ) ;
#5866 = DIRECTION ( 'NONE',  ( 1.000000000000000000, 8.881784197001244435E-16, 0.000000000000000000 ) ) ;
#5867 = VERTEX_POINT ( 'NONE', #1673 ) ;
#5868 = CONICAL_SURFACE ( 'NONE', #5005, 8.000000000000007105, 1.047197551196597631 ) ;
#5869 = CARTESIAN_POINT ( 'NONE',  ( 0.000000000000000000, 0.000000000000000000, -8.400999999999992696 ) ) ;
#5870 = CIRCLE ( 'NONE', #5136, 5.499999999999999112 ) ;
#5871 = CIRCLE ( 'NONE', #2100, 4.250000000000007105 ) ;
#5872 = PRODUCT ( 'hex nut style 1_am_B18.2.4.1M - Hex nut, Style 1,  M10 x 1.5, with 16mm WAF --D-N', 'hex nut style 1_am_B18.2.4.1M - Hex nut, Style 1,  M10 x 1.5, with 16mm WAF --D-N', '', ( #4452 ) ) ;
#5873 = EDGE_CURVE ( 'NONE', #2950, #1229, #2232, .T. ) ;
#5874 = DIRECTION ( 'NONE',  ( -1.058471975245261993E-16, 8.736544766236848795E-16, -1.000000000000000000 ) ) ;
#5875 = AXIS2_PLACEMENT_3D ( 'NONE', #4784, #5484, #4695 ) ;
#5876 = CIRCLE ( 'NONE', #287, 75.00000000000000000 ) ;
#5877 = CARTESIAN_POINT ( 'NONE',  ( -8.000000000000229150, -4.618802153516843312, -7.685468820183672278 ) ) ;
#5878 = ORIENTED_EDGE ( 'NONE', *, *, #3401, .F. ) ;
#5879 = LINE ( 'NONE', #2722, #1404 ) ;
#5880 = ADVANCED_FACE ( 'NONE', ( #1155 ), #1078, .T. ) ;
#5881 = ORIENTED_EDGE ( 'NONE', *, *, #5016, .T. ) ;
#5882 = CARTESIAN_POINT ( 'NONE',  ( -6.661338147750939243E-13, 9.237604307034352757, -0.7145311798163467287 ) ) ;
#5883 = ORIENTED_EDGE ( 'NONE', *, *, #7319, .F. ) ;
#5884 = CARTESIAN_POINT ( 'NONE',  ( 6.689127551062092891, 5.375634714784657930, -8.082649155111312211 ) ) ;
#5885 = CARTESIAN_POINT ( 'NONE',  ( 0.000000000000000000, 9.237604307034130713, 0.000000000000000000 ) ) ;
#5886 = CARTESIAN_POINT ( 'NONE',  ( 2.220446049250313081E-13, -9.237604307034242623, -8.400000000000018119 ) ) ;
#5887 = CARTESIAN_POINT ( 'NONE',  ( 1.110223024625156540E-13, 9.237604307033992157, -0.7145311798163467287 ) ) ;
#5888 = DIRECTION ( 'NONE',  ( 0.000000000000000000, 0.000000000000000000, 1.000000000000000000 ) ) ;
#5889 = EDGE_CURVE ( 'NONE', #6735, #6221, #5111, .T. ) ;
#5890 = PRODUCT_RELATED_PRODUCT_CATEGORY ( 'part', '', ( #2728 ) ) ;
#5891 = DIRECTION ( 'NONE',  ( 6.400024471206996205E-36, -1.000000000000000000, -7.598173571352216173E-18 ) ) ;
#5892 = ORIENTED_EDGE ( 'NONE', *, *, #7710, .T. ) ;
#5893 = DIRECTION ( 'NONE',  ( 3.919652622816902408E-30, 3.944304526105059027E-30, -1.000000000000000000 ) ) ;
#5894 = EDGE_LOOP ( 'NONE', ( #557, #847, #4997, #373 ) ) ;
#5895 = LINE ( 'NONE', #4656, #1760 ) ;
#5896 = SURFACE_STYLE_FILL_AREA ( #6701 ) ;
#5897 = ADVANCED_FACE ( 'NONE', ( #6362 ), #7661, .T. ) ;
#5898 = CARTESIAN_POINT ( 'NONE',  ( 10.00000000000000888, -650.0000000000002274, -1.110223024625156540E-13 ) ) ;
#5899 = ITEM_DEFINED_TRANSFORMATION ( 'NONE', 'NONE', #752,  #7563 ) ;
#5900 = EDGE_LOOP ( 'NONE', ( #906, #4736 ) ) ;
#5901 = DIRECTION ( 'NONE',  ( 0.000000000000000000, -1.000000000000000000, -1.224646799147352714E-16 ) ) ;
#5902 = VERTEX_POINT ( 'NONE', #8393 ) ;
#5903 = VERTEX_POINT ( 'NONE', #5842 ) ;
#5904 = CIRCLE ( 'NONE', #4907, 8.000000000000007105 ) ;
#5905 = DIRECTION ( 'NONE',  ( -1.000000000000000000, 1.774937036747276562E-30, 0.000000000000000000 ) ) ;
#5906 = VERTEX_POINT ( 'NONE', #2422 ) ;
#5907 = AXIS2_PLACEMENT_3D ( 'NONE', #6784, #2168, #7473 ) ;
#5908 = CARTESIAN_POINT ( 'NONE',  ( -5.355005115541073835, -6.145890662064625865, -8.317753204360252894 ) ) ;
#5909 = CARTESIAN_POINT ( 'NONE',  ( 0.7999999999999674039, 6.779273404243070203E-29, -6.499999999999968026 ) ) ;
#5910 = AXIS2_PLACEMENT_3D ( 'NONE', #3916, #2615, #3756 ) ;
#5911 = AXIS2_PLACEMENT_3D ( 'NONE', #2575, #5863, #2479 ) ;
#5912 = CYLINDRICAL_SURFACE ( 'NONE', #7689, 5.500000000000000000 ) ;
#5913 = DIRECTION ( 'NONE',  ( 3.549874073494553825E-30, -1.000000000000000000, 1.478898702612476446E-15 ) ) ;
#5914 = ORIENTED_EDGE ( 'NONE', *, *, #1302, .T. ) ;
#5915 = DIRECTION ( 'NONE',  ( -1.463706757734299248E-32, 1.000000000000000000, 5.238529448733281520E-32 ) ) ;
#5916 = VECTOR ( 'NONE', #7197, 1000.000000000000114 ) ;
#5917 = ADVANCED_FACE ( 'NONE', ( #7085 ), #8376, .T. ) ;
#5918 = AXIS2_PLACEMENT_3D ( 'NONE', #8512, #2514, #3740 ) ;
#5919 = CARTESIAN_POINT ( 'NONE',  ( 0.000000000000000000, 0.000000000000000000, -8.400000000000018119 ) ) ;
#5920 = VERTEX_POINT ( 'NONE', #6433 ) ;
#5921 = CARTESIAN_POINT ( 'NONE',  ( -82.49999999999945999, 120.0000000000003268, 10.00000000000000888 ) ) ;
#5922 =( NAMED_UNIT ( * ) SI_UNIT ( $, .STERADIAN. ) SOLID_ANGLE_UNIT ( ) );
#5923 = VERTEX_POINT ( 'NONE', #3161 ) ;
#5924 = DIRECTION ( 'NONE',  ( -3.851859888774471706E-33, -1.232595164407830946E-32, -1.000000000000000000 ) ) ;
#5925 = ORIENTED_EDGE ( 'NONE', *, *, #1434, .T. ) ;
#5926 = CARTESIAN_POINT ( 'NONE',  ( -7.347286611336995676, -4.995646404165323240, -0.4969600502617779747 ) ) ;
#5927 = ADVANCED_FACE ( 'NONE', ( #470 ), #1809, .T. ) ;
#5928 = EDGE_CURVE ( 'NONE', #7472, #7867, #5250, .T. ) ;
#5929 = FACE_OUTER_BOUND ( 'NONE', #7205, .T. ) ;
#5930 = PRODUCT_DEFINITION_FORMATION_WITH_SPECIFIED_SOURCE ( 'ANY', '', #5800, .NOT_KNOWN. ) ;
#5931 = DIRECTION ( 'NONE',  ( -1.000000000000000000, 3.549874073494553124E-30, 0.000000000000000000 ) ) ;
#5932 = DIRECTION ( 'NONE',  ( -1.463706757734299248E-32, 1.000000000000000000, 5.238529448733281520E-32 ) ) ;
#5933 = CARTESIAN_POINT ( 'NONE',  ( -4.391120273202894942E-30, 295.0000000000000568, 74.99999999999995737 ) ) ;
#5934 = ORIENTED_EDGE ( 'NONE', *, *, #69, .T. ) ;
#5935 = PRESENTATION_STYLE_ASSIGNMENT (( #7091 ) ) ;
#5936 = ORIENTED_EDGE ( 'NONE', *, *, #5821, .T. ) ;
#5937 = DIRECTION ( 'NONE',  ( -1.000000000000000000, -8.881784197001244435E-16, 0.000000000000000000 ) ) ;
#5938 = ADVANCED_FACE ( 'NONE', ( #3330 ), #7949, .F. ) ;
#5939 = PRODUCT ( 'Conveyor belt', 'Conveyor belt', '', ( #37 ) ) ;
#5940 = DIRECTION ( 'NONE',  ( 3.851859888774471706E-33, -7.598173571352220795E-18, 1.000000000000000000 ) ) ;
#5941 = ORIENTED_EDGE ( 'NONE', *, *, #5873, .F. ) ;
#5942 = ADVANCED_FACE ( 'NONE', ( #1938 ), #418, .T. ) ;
#5943 = DIRECTION ( 'NONE',  ( -0.000000000000000000, -0.000000000000000000, 1.000000000000000000 ) ) ;
#5944 = EDGE_LOOP ( 'NONE', ( #1500, #68, #946, #4514 ) ) ;
#5945 = ORIENTED_EDGE ( 'NONE', *, *, #6968, .F. ) ;
#5946 = DIRECTION ( 'NONE',  ( 6.400024471206993532E-36, -1.000000000000000000, -7.598173571352213092E-18 ) ) ;
#5947 = ORIENTED_EDGE ( 'NONE', *, *, #3586, .T. ) ;
#5948 = CARTESIAN_POINT ( 'NONE',  ( -4.681481898397863439, 6.534749472788354829, -3.895114889266789776E-13 ) ) ;
#5949 = ADVANCED_BREP_SHAPE_REPRESENTATION ( '', ( #5730, #7563 ), #6881 ) ;
#5950 = CARTESIAN_POINT ( 'NONE',  ( -3.660532965669041516, 7.124194613927598674, -4.381983780462242249E-14 ) ) ;
#5951 = PLANE ( 'NONE',  #5192 ) ;
#5952 = FACE_OUTER_BOUND ( 'NONE', #6117, .T. ) ;
#5953 = ORIENTED_EDGE ( 'NONE', *, *, #8008, .T. ) ;
#5954 = CARTESIAN_POINT ( 'NONE',  ( 32.49999999999997158, 1.387778780781445676E-14, 18.00000000000000355 ) ) ;
#5955 = APPLICATION_PROTOCOL_DEFINITION ( 'draft international standard', 'automotive_design', 1998, #5779 ) ;
#5956 = ORIENTED_EDGE ( 'NONE', *, *, #7467, .F. ) ;
#5957 = FACE_OUTER_BOUND ( 'NONE', #1929, .T. ) ;
#5958 = DIRECTION ( 'NONE',  ( 0.000000000000000000, -0.000000000000000000, 1.000000000000000000 ) ) ;
#5959 = ORIENTED_EDGE ( 'NONE', *, *, #1647, .T. ) ;
#5960 = EDGE_CURVE ( 'NONE', #3289, #5332, #4029, .T. ) ;
#5961 = CARTESIAN_POINT ( 'NONE',  ( 5.355005115540884653, 6.145890662064626753, -8.317753204360318620 ) ) ;
#5962 = ORIENTED_EDGE ( 'NONE', *, *, #3824, .F. ) ;
#5963 = FACE_OUTER_BOUND ( 'NONE', #2910, .T. ) ;
#5964 = CARTESIAN_POINT ( 'NONE',  ( 3.660532965668862992, -7.124194613927656405, -8.399999999999993250 ) ) ;
#5965 = CARTESIAN_POINT ( 'NONE',  ( 0.000000000000000000, -3.469446951953614189E-15, 130.0000000000000000 ) ) ;
#5966 = DIRECTION ( 'NONE',  ( 0.7071067811865483499, 5.015942853700631228E-30, -0.7071067811865467956 ) ) ;
#5967 = CARTESIAN_POINT ( 'NONE',  ( -5.690023276062574631, -5.952467836904122400, -0.1306530452038688617 ) ) ;
#5968 = ORIENTED_EDGE ( 'NONE', *, *, #4528, .F. ) ;
#5969 = EDGE_CURVE ( 'NONE', #2630, #7000, #1798, .T. ) ;
#5970 = CARTESIAN_POINT ( 'NONE',  ( -8.000000000000117240, -1.110223024625156540E-13, 0.000000000000000000 ) ) ;
#5971 = ORIENTED_EDGE ( 'NONE', *, *, #7429, .T. ) ;
#5972 = DIRECTION ( 'NONE',  ( 0.000000000000000000, 0.000000000000000000, 1.000000000000000000 ) ) ;
#5973 =( REPRESENTATION_RELATIONSHIP ('NONE','NONE', #1279, #6969 ) REPRESENTATION_RELATIONSHIP_WITH_TRANSFORMATION ( #6108 )SHAPE_REPRESENTATION_RELATIONSHIP( ) );
#5974 = CARTESIAN_POINT ( 'NONE',  ( 0.000000000000000000, -299.9999999999999432, 24.49999999999997158 ) ) ;
#5975 = DIRECTION ( 'NONE',  ( -1.000000000000000000, 1.284024588418159817E-35, 0.000000000000000000 ) ) ;
#5976 = DIRECTION ( 'NONE',  ( 0.000000000000000000, 0.000000000000000000, 1.000000000000000000 ) ) ;
#5977 = DIRECTION ( 'NONE',  ( 0.000000000000000000, -4.930380657631321594E-32, -1.000000000000000000 ) ) ;
#5978 = ITEM_DEFINED_TRANSFORMATION ( 'NONE', 'NONE', #5200,  #7563 ) ;
#5979 = CARTESIAN_POINT ( 'NONE',  ( -4.000000000000003553, 6.928203230275209457, -8.400000000000018119 ) ) ;
#5980 = DIRECTION ( 'NONE',  ( 0.000000000000000000, 0.000000000000000000, -1.000000000000000000 ) ) ;
#5981 = ORIENTED_EDGE ( 'NONE', *, *, #5428, .F. ) ;
#5982 = ADVANCED_FACE ( 'NONE', ( #7860 ), #5168, .T. ) ;
#5983 = CARTESIAN_POINT ( 'NONE',  ( 6.686525924292749501, -5.377136764700527927, -0.3167204509599568785 ) ) ;
#5984 = ORIENTED_EDGE ( 'NONE', *, *, #2217, .T. ) ;
#5985 = DIRECTION ( 'NONE',  ( -1.000000000000000000, 3.549874073494553124E-30, 3.778304382545602261E-59 ) ) ;
#5986 = ORIENTED_EDGE ( 'NONE', *, *, #5252, .F. ) ;
#5987 = DIRECTION ( 'NONE',  ( 1.000000000000000000, 0.000000000000000000, 0.000000000000000000 ) ) ;
#5988 = APPLICATION_CONTEXT ( 'automotive_design' ) ;
#5989 = VECTOR ( 'NONE', #4474, 1000.000000000000227 ) ;
#5990 = DIRECTION ( 'NONE',  ( 1.540743955509788340E-33, -6.569728034446847052E-68, 1.000000000000000000 ) ) ;
#5991 = LINE ( 'NONE', #2613, #883 ) ;
#5992 = CARTESIAN_POINT ( 'NONE',  ( -8.000000000000007105, 1.110223024625156540E-13, -8.400000000000018119 ) ) ;
#5993 = DIRECTION ( 'NONE',  ( 0.000000000000000000, 0.000000000000000000, 1.000000000000000000 ) ) ;
#5994 = ORIENTED_EDGE ( 'NONE', *, *, #5444, .F. ) ;
#5995 = EDGE_CURVE ( 'NONE', #6892, #8044, #1422, .T. ) ;
#5996 = PRODUCT_CONTEXT ( 'NONE', #2157, 'mechanical' ) ;
#5997 = AXIS2_PLACEMENT_3D ( 'NONE', #1615, #5655, #4148 ) ;
#5998 = AXIS2_PLACEMENT_3D ( 'NONE', #3210, #4740, #1202 ) ;
#5999 = AXIS2_PLACEMENT_3D ( 'NONE', #756, #3414, #7548 ) ;
#6000 = VERTEX_POINT ( 'NONE', #5388 ) ;
#6001 = CLOSED_SHELL ( 'NONE', ( #4106, #5294, #684, #8494, #6952, #1755, #4198, #2519, #8547, #1077 ) ) ;
#6002 = CARTESIAN_POINT ( 'NONE',  ( 2.645508037661955303, 7.710219529346675316, -0.06809871960547979330 ) ) ;
#6003 = CIRCLE ( 'NONE', #7789, 3.047499999999999876 ) ;
#6004 = EDGE_LOOP ( 'NONE', ( #4783, #3685, #3498, #2186, #2367 ) ) ;
#6005 = EDGE_CURVE ( 'NONE', #6260, #7754, #4649, .T. ) ;
#6006 = AXIS2_PLACEMENT_3D ( 'NONE', #8359, #4914, #348 ) ;
#6007 = CARTESIAN_POINT ( 'NONE',  ( -8.000000000000007105, 1.110223024625156540E-13, 0.000000000000000000 ) ) ;
#6008 = EDGE_LOOP ( 'NONE', ( #6258, #4161 ) ) ;
#6009 =( GEOMETRIC_REPRESENTATION_CONTEXT ( 3 ) GLOBAL_UNCERTAINTY_ASSIGNED_CONTEXT ( ( #7441 ) ) GLOBAL_UNIT_ASSIGNED_CONTEXT ( ( #5032, #2333, #3697 ) ) REPRESENTATION_CONTEXT ( 'NONE', 'WORKASPACE' ) );
#6010 = ADVANCED_FACE ( 'NONE', ( #3282 ), #3245, .F. ) ;
#6011 = DIRECTION ( 'NONE',  ( 0.000000000000000000, -5.322451846059955323E-30, 1.000000000000000000 ) ) ;
#6012 = DIRECTION ( 'NONE',  ( 3.919652622816902408E-30, 3.944304526105059027E-30, -1.000000000000000000 ) ) ;
#6013 = LINE ( 'NONE', #5251, #3616 ) ;
#6014 = FACE_OUTER_BOUND ( 'NONE', #6286, .T. ) ;
#6015 = CARTESIAN_POINT ( 'NONE',  ( -4.680456609904114273, -6.535341423375586878, -0.01688885742781164739 ) ) ;
#6016 = ORIENTED_EDGE ( 'NONE', *, *, #732, .F. ) ;
#6017 = DIRECTION ( 'NONE',  ( -3.851859888774471706E-33, -1.232595164407830946E-32, -1.000000000000000000 ) ) ;
#6018 = DIRECTION ( 'NONE',  ( -0.000000000000000000, -0.000000000000000000, 1.000000000000000000 ) ) ;
#6019 = CARTESIAN_POINT ( 'NONE',  ( 8.000000000000117240, 4.618802153516954334, -8.400000000000018119 ) ) ;
#6020 = EDGE_CURVE ( 'NONE', #7803, #2390, #5143, .T. ) ;
#6021 = CONTEXT_DEPENDENT_SHAPE_REPRESENTATION ( #5524, #4104 ) ;
#6022 = DIRECTION ( 'NONE',  ( -1.000000000000000000, 3.549874073494553124E-30, 0.000000000000000000 ) ) ;
#6023 = CARTESIAN_POINT ( 'NONE',  ( -8.000000000000673239, 4.618802153517287401, -8.400000000000018119 ) ) ;
#6024 = ORIENTED_EDGE ( 'NONE', *, *, #952, .T. ) ;
#6025 = LINE ( 'NONE', #5360, #4176 ) ;
#6026 = ORIENTED_EDGE ( 'NONE', *, *, #5180, .T. ) ;
#6027 = CARTESIAN_POINT ( 'NONE',  ( -3.318518101603130876, -7.321656987762883873, -8.399999999999986144 ) ) ;
#6028 = VERTEX_POINT ( 'NONE', #6059 ) ;
#6029 = VECTOR ( 'NONE', #5931, 1000.000000000000000 ) ;
#6030 = CARTESIAN_POINT ( 'NONE',  ( -4.000000000000891731, 6.928203230275542523, 0.000000000000000000 ) ) ;
#6031 = CARTESIAN_POINT ( 'NONE',  ( -1.310872448938079859, 8.480771745766464420, -0.3173508448886962485 ) ) ;
#6032 = CARTESIAN_POINT ( 'NONE',  ( 1.140226871204266778E-13, -410.0000000000000568, -24.50000000000006750 ) ) ;
#6033 = ADVANCED_FACE ( 'NONE', ( #4602 ), #8041, .T. ) ;
#6034 = FACE_OUTER_BOUND ( 'NONE', #995, .T. ) ;
#6035 = PLANE ( 'NONE',  #3086 ) ;
#6036 = ORIENTED_EDGE ( 'NONE', *, *, #485, .F. ) ;
#6037 = DIRECTION ( 'NONE',  ( -0.8660254037844362651, -0.5000000000000039968, 0.000000000000000000 ) ) ;
#6038 = ORIENTED_EDGE ( 'NONE', *, *, #7761, .F. ) ;
#6039 = SHAPE_DEFINITION_REPRESENTATION ( #6772, #2536 ) ;
#6040 = VECTOR ( 'NONE', #8551, 1000.000000000000000 ) ;
#6041 = CIRCLE ( 'NONE', #7553, 24.50000000000001066 ) ;
#6042 = CIRCLE ( 'NONE', #7269, 8.000000000000007105 ) ;
#6043 = EDGE_CURVE ( 'NONE', #704, #683, #3200, .T. ) ;
#6044 = LINE ( 'NONE', #2719, #6517 ) ;
#6045 = ORIENTED_EDGE ( 'NONE', *, *, #6867, .F. ) ;
#6046 = LINE ( 'NONE', #7848, #1113 ) ;
#6047 = VECTOR ( 'NONE', #8137, 1000.000000000000000 ) ;
#6048 =( NAMED_UNIT ( * ) SI_UNIT ( $, .STERADIAN. ) SOLID_ANGLE_UNIT ( ) );
#6049 = ORIENTED_EDGE ( 'NONE', *, *, #4265, .T. ) ;
#6050 = VECTOR ( 'NONE', #6713, 1000.000000000000000 ) ;
#6051 = EDGE_CURVE ( 'NONE', #3105, #7042, #7298, .T. ) ;
#6052 = LINE ( 'NONE', #2727, #3092 ) ;
#6053 = ORIENTED_EDGE ( 'NONE', *, *, #4982, .F. ) ;
#6054 = AXIS2_PLACEMENT_3D ( 'NONE', #6532, #5990, #1823 ) ;
#6055 = LINE ( 'NONE', #4548, #876 ) ;
#6056 = AXIS2_PLACEMENT_3D ( 'NONE', #8229, #7573, #292 ) ;
#6057 = CIRCLE ( 'NONE', #8121, 8.000000000000007105 ) ;
#6058 = DIRECTION ( 'NONE',  ( 0.000000000000000000, 0.000000000000000000, 1.000000000000000000 ) ) ;
#6059 = CARTESIAN_POINT ( 'NONE',  ( 1.224646799147351679E-15, -9.499999999999984013, 130.0000000000000000 ) ) ;
#6060 = DIRECTION ( 'NONE',  ( 1.000000000000000000, 8.881784197001244435E-16, 0.000000000000000000 ) ) ;
#6061 = CARTESIAN_POINT ( 'NONE',  ( 8.000000000000124345, -3.867591403079279733, -0.4976753153246756822 ) ) ;
#6062 = AXIS2_PLACEMENT_3D ( 'NONE', #933, #2164, #6132 ) ;
#6063 = CARTESIAN_POINT ( 'NONE',  ( -6.661338147750939243E-13, -9.237604307034130713, -8.400000000000018119 ) ) ;
#6064 = ORIENTED_EDGE ( 'NONE', *, *, #498, .T. ) ;
#6065 = PLANE ( 'NONE',  #3493 ) ;
#6066 = CARTESIAN_POINT ( 'NONE',  ( -2.220446049250313081E-13, -650.0000000000000000, -1.110223024625156540E-13 ) ) ;
#6067 = DIRECTION ( 'NONE',  ( -1.000000000000000000, 2.842664852890546338E-35, 1.540743955509788340E-33 ) ) ;
#6068 = CONTEXT_DEPENDENT_SHAPE_REPRESENTATION ( #6853, #4250 ) ;
#6069 = CARTESIAN_POINT ( 'NONE',  ( 5.000000000000115463, 3.513898075855330205, -2.028750000000023590 ) ) ;
#6070 = CARTESIAN_POINT ( 'NONE',  ( -8.000000000000229150, 4.618802153516954334, -7.685468820183672278 ) ) ;
#6071 = EDGE_LOOP ( 'NONE', ( #1048, #7437 ) ) ;
#6072 = ORIENTED_EDGE ( 'NONE', *, *, #4022, .T. ) ;
#6073 = B_SPLINE_CURVE_WITH_KNOTS ( 'NONE', 3,
 ( #7275, #5950, #3402, #4005, #1311, #6031, #28, #7621 ),
 .UNSPECIFIED., .F., .F.,
 ( 4, 2, 2, 4 ),
 ( 0.004673709593152869553, 0.005837709341828219330, 0.007001709090503569974, 0.009329708587854271262 ),
 .UNSPECIFIED. ) ;
#6074 = EDGE_CURVE ( 'NONE', #7841, #1496, #7997, .T. ) ;
#6075 = CARTESIAN_POINT ( 'NONE',  ( -2.645508037662052558, -7.710219529346595380, -8.331901280394566456 ) ) ;
#6076 = ORIENTED_EDGE ( 'NONE', *, *, #4763, .T. ) ;
#6077 = CARTESIAN_POINT ( 'NONE',  ( 5.759474945355391284, 1.387778780781445676E-14, 0.000000000000000000 ) ) ;
#6078 = CARTESIAN_POINT ( 'NONE',  ( 5.000000000000060396, -2.342598717236958006, -4.057500000000047180 ) ) ;
#6079 = PLANE ( 'NONE',  #5183 ) ;
#6080 = ORIENTED_EDGE ( 'NONE', *, *, #1266, .T. ) ;
#6081 = AXIS2_PLACEMENT_3D ( 'NONE', #6478, #3707, #8521 ) ;
#6082 = ORIENTED_EDGE ( 'NONE', *, *, #2607, .F. ) ;
#6083 = PRODUCT_DEFINITION_SHAPE ( 'NONE', 'NONE',  #8613 ) ;
#6084 = VECTOR ( 'NONE', #7253, 1000.000000000000000 ) ;
#6085 = EDGE_CURVE ( 'NONE', #7727, #6135, #2027, .T. ) ;
#6086 = CARTESIAN_POINT ( 'NONE',  ( 0.000000000000000000, -299.9999999999999432, -2.775557561562891351E-14 ) ) ;
#6087 = CARTESIAN_POINT ( 'NONE',  ( 0.000000000000000000, 0.000000000000000000, 0.000000000000000000 ) ) ;
#6088 = EDGE_LOOP ( 'NONE', ( #1638, #3949, #6942 ) ) ;
#6089 = CARTESIAN_POINT ( 'NONE',  ( 36.74999999999998579, 1.439826269745208429E-14, 18.00000000000000355 ) ) ;
#6090 = VERTEX_POINT ( 'NONE', #588 ) ;
#6091 =( REPRESENTATION_RELATIONSHIP ('NONE','NONE', #1279, #3167 ) REPRESENTATION_RELATIONSHIP_WITH_TRANSFORMATION ( #4354 )SHAPE_REPRESENTATION_RELATIONSHIP( ) );
#6092 = EDGE_CURVE ( 'NONE', #4339, #5835, #1373, .T. ) ;
#6093 = CARTESIAN_POINT ( 'NONE',  ( 7.347286611336940609, 4.995646404165252186, -7.903039949738288605 ) ) ;
#6094 = ORIENTED_EDGE ( 'NONE', *, *, #7084, .T. ) ;
#6095 = DIRECTION ( 'NONE',  ( 0.000000000000000000, 0.000000000000000000, 1.000000000000000000 ) ) ;
#6096 = CIRCLE ( 'NONE', #7481, 8.000000000000007105 ) ;
#6097 = CARTESIAN_POINT ( 'NONE',  ( 0.000000000000000000, 2.342598717236902939, 4.057500000000047180 ) ) ;
#6098 = ORIENTED_EDGE ( 'NONE', *, *, #5607, .T. ) ;
#6099 = CARTESIAN_POINT ( 'NONE',  ( 50.00000000000004263, -500.0000000000000000, 45.00000000000000711 ) ) ;
#6100 = CARTESIAN_POINT ( 'NONE',  ( 8.000000000000012434, 0.7809653281572520589, -8.400000000000034106 ) ) ;
#6101 = CARTESIAN_POINT ( 'NONE',  ( -8.000000000000667910, 3.115336682267232593, -0.3193931313919167181 ) ) ;
#6102 = FACE_OUTER_BOUND ( 'NONE', #4963, .T. ) ;
#6103 = EDGE_LOOP ( 'NONE', ( #3730, #7066 ) ) ;
#6104 = DIRECTION ( 'NONE',  ( 0.000000000000000000, 0.000000000000000000, 1.000000000000000000 ) ) ;
#6105 = ORIENTED_EDGE ( 'NONE', *, *, #7570, .F. ) ;
#6106 = CARTESIAN_POINT ( 'NONE',  ( 5.080504117408890075, 2.106769544347818268, -8.400000000000018119 ) ) ;
#6107 = CARTESIAN_POINT ( 'NONE',  ( -7.345652830558694113, 4.996589667937325174, -0.4964154566687435377 ) ) ;
#6108 = ITEM_DEFINED_TRANSFORMATION ( 'NONE', 'NONE', #4801,  #7563 ) ;
#6109 = DIRECTION ( 'NONE',  ( 3.919652622816902408E-30, 3.944304526105059027E-30, -1.000000000000000000 ) ) ;
#6110 = CARTESIAN_POINT ( 'NONE',  ( -50.00000000000004263, -425.0000000000000000, -25.00000000000000355 ) ) ;
#6111 = ORIENTED_EDGE ( 'NONE', *, *, #1704, .T. ) ;
#6112 = DIRECTION ( 'NONE',  ( 3.851859888774471706E-33, 1.232595164407830946E-32, 1.000000000000000000 ) ) ;
#6113 = VERTEX_POINT ( 'NONE', #5054 ) ;
#6114 = DIRECTION ( 'NONE',  ( -1.000000000000000000, 0.000000000000000000, 6.938893903907228378E-17 ) ) ;
#6115 = CARTESIAN_POINT ( 'NONE',  ( -7.345652830559441071, 4.996589667937682222, -0.4964154566692197679 ) ) ;
#6116 = DIRECTION ( 'NONE',  ( -1.000000000000000000, 0.000000000000000000, 6.938893903907228378E-17 ) ) ;
#6117 = EDGE_LOOP ( 'NONE', ( #3186, #3047, #7061 ) ) ;
#6118 = DIRECTION ( 'NONE',  ( 0.000000000000000000, -1.213383262747659708E-29, 1.000000000000000000 ) ) ;
#6119 = EDGE_CURVE ( 'NONE', #7090, #3424, #1277, .T. ) ;
#6120 = ORIENTED_EDGE ( 'NONE', *, *, #6695, .T. ) ;
#6121 = ORIENTED_EDGE ( 'NONE', *, *, #7719, .T. ) ;
#6122 = SHAPE_REPRESENTATION ( 'Flipper', ( #7563 ), #4918 ) ;
#6123 = CIRCLE ( 'NONE', #5423, 6.500000000000000888 ) ;
#6124 = VECTOR ( 'NONE', #3363, 1000.000000000000114 ) ;
#6125 = AXIS2_PLACEMENT_3D ( 'NONE', #5035, #8471, #545 ) ;
#6126 = DIRECTION ( 'NONE',  ( -0.000000000000000000, -0.000000000000000000, 1.000000000000000000 ) ) ;
#6127 = ADVANCED_FACE ( 'NONE', ( #1018 ), #3053, .T. ) ;
#6128 = ORIENTED_EDGE ( 'NONE', *, *, #494, .F. ) ;
#6129 = VECTOR ( 'NONE', #1127, 1000.000000000000000 ) ;
#6130 = FACE_OUTER_BOUND ( 'NONE', #5232, .T. ) ;
#6131 = DIRECTION ( 'NONE',  ( -1.000000000000000000, 3.549874073494553124E-30, -0.000000000000000000 ) ) ;
#6132 = DIRECTION ( 'NONE',  ( 0.000000000000000000, 0.000000000000000000, 1.000000000000000000 ) ) ;
#6133 = ORIENTED_EDGE ( 'NONE', *, *, #5705, .T. ) ;
#6134 = AXIS2_PLACEMENT_3D ( 'NONE', #6225, #2894, #283 ) ;
#6135 = VERTEX_POINT ( 'NONE', #309 ) ;
#6136 = CARTESIAN_POINT ( 'NONE',  ( -34.92499999999998295, 0.000000000000000000, 0.000000000000000000 ) ) ;
#6137 = VECTOR ( 'NONE', #4889, 1000.000000000000000 ) ;
#6138 = B_SPLINE_CURVE_WITH_KNOTS ( 'NONE', 3,
 ( #3934, #582, #1228, #6428, #7899, #503 ),
 .UNSPECIFIED., .F., .F.,
 ( 4, 2, 4 ),
 ( 2.380731630400558434E-07, 0.002336973833157513902, 0.004673709593151988313 ),
 .UNSPECIFIED. ) ;
#6139 = DIRECTION ( 'NONE',  ( 0.8660254037844367092, -0.5000000000000033307, 0.000000000000000000 ) ) ;
#6140 = EDGE_CURVE ( 'NONE', #316, #758, #4238, .T. ) ;
#6142 = VERTEX_POINT ( 'NONE', #8286 ) ;
#6141 = VECTOR ( 'NONE', #6700, 1000.000000000000000 ) ;
#6143 = PRODUCT_DEFINITION_SHAPE ( 'NONE', 'NONE',  #8622 ) ;
#6144 = DIRECTION ( 'NONE',  ( 0.000000000000000000, -0.000000000000000000, 1.000000000000000000 ) ) ;
#6145 = DIRECTION ( 'NONE',  ( -7.703719777548943412E-34, 0.000000000000000000, 1.000000000000000000 ) ) ;
#6146 = AXIS2_PLACEMENT_3D ( 'NONE', #3611, #2297, #1044 ) ;
#6147 = ORIENTED_EDGE ( 'NONE', *, *, #5052, .T. ) ;
#6148 = CIRCLE ( 'NONE', #3759, 15.00000000000000355 ) ;
#6149 =( NAMED_UNIT ( * ) SI_UNIT ( $, .STERADIAN. ) SOLID_ANGLE_UNIT ( ) );
#6150 = CARTESIAN_POINT ( 'NONE',  ( -4.339467034331259576, -6.732211846623360252, -9.205130554286108935E-16 ) ) ;
#6151 = CARTESIAN_POINT ( 'NONE',  ( -21.99999999999955946, 120.0000000000003126, 9.999999999999980460 ) ) ;
#6152 = EDGE_CURVE ( 'NONE', #6090, #4173, #1058, .T. ) ;
#6153 = CARTESIAN_POINT ( 'NONE',  ( 0.000000000000000000, 0.000000000000000000, 10.00000000000000888 ) ) ;
#6154 = CARTESIAN_POINT ( 'NONE',  ( 0.000000000000000000, 0.000000000000000000, -8.400999999999992696 ) ) ;
#6155 = ORIENTED_EDGE ( 'NONE', *, *, #7725, .T. ) ;
#6156 = LINE ( 'NONE', #6803, #7783 ) ;
#6157 = ORIENTED_EDGE ( 'NONE', *, *, #2663, .T. ) ;
#6158 = CARTESIAN_POINT ( 'NONE',  ( -3.318518101603001647, -7.321656987763291546, -2.234845609353635682E-13 ) ) ;
#6159 = CARTESIAN_POINT ( 'NONE',  ( -45.49999999999945999, 152.5000000000003126, 9.999999999999786837 ) ) ;
#6160 = CARTESIAN_POINT ( 'NONE',  ( -44.99999999999992895, 500.0000000000000000, 45.00000000000000711 ) ) ;
#6161 = ORIENTED_EDGE ( 'NONE', *, *, #3303, .T. ) ;
#6162 = FACE_BOUND ( 'NONE', #6720, .T. ) ;
#6163 = ORIENTED_EDGE ( 'NONE', *, *, #1342, .F. ) ;
#6164 = CARTESIAN_POINT ( 'NONE',  ( -36.74999999999997868, 3.469446951953614189E-15, 18.00000000000000355 ) ) ;
#6165 = ORIENTED_EDGE ( 'NONE', *, *, #7073, .F. ) ;
#6166 = EDGE_CURVE ( 'NONE', #2122, #6377, #8277, .T. ) ;
#6167 = FILL_AREA_STYLE ('',( #2718 ) ) ;
#6168 = DIRECTION ( 'NONE',  ( 0.000000000000000000, 0.000000000000000000, 1.000000000000000000 ) ) ;
#6169 = CIRCLE ( 'NONE', #6855, 5.000000000000034639 ) ;
#6170 = ORIENTED_EDGE ( 'NONE', *, *, #7134, .F. ) ;
#6171 = VECTOR ( 'NONE', #1189, 1000.000000000000114 ) ;
#6172 = DIRECTION ( 'NONE',  ( 0.000000000000000000, 0.000000000000000000, 1.000000000000000000 ) ) ;
#6173 = DIRECTION ( 'NONE',  ( 0.000000000000000000, -1.795949010423047374E-16, 1.000000000000000000 ) ) ;
#6174 = DIRECTION ( 'NONE',  ( 1.692239235979712873E-17, -0.1547107621133612942, 0.9879598069184307718 ) ) ;
#6175 = VERTEX_POINT ( 'NONE', #7672 ) ;
#6176 = CARTESIAN_POINT ( 'NONE',  ( 0.000000000000000000, 0.000000000000000000, 0.000000000000000000 ) ) ;
#6177 = AXIS2_PLACEMENT_3D ( 'NONE', #6597, #8080, #7379 ) ;
#6178 = ORIENTED_EDGE ( 'NONE', *, *, #4473, .T. ) ;
#6179 = DIRECTION ( 'NONE',  ( -1.000000000000000000, 3.549874073494553124E-30, 0.000000000000000000 ) ) ;
#6180 = EDGE_CURVE ( 'NONE', #2313, #4294, #5376, .T. ) ;
#6181 = DIRECTION ( 'NONE',  ( -1.000000000000000000, -2.664535259100374908E-15, 0.000000000000000000 ) ) ;
#6182 = ORIENTED_EDGE ( 'NONE', *, *, #2437, .T. ) ;
#6183 = AXIS2_PLACEMENT_3D ( 'NONE', #4534, #6534, #8576 ) ;
#6184 = VECTOR ( 'NONE', #6579, 1000.000000000000000 ) ;
#6185 = CARTESIAN_POINT ( 'NONE',  ( 5.080504117408895404, 2.106769544347820489, -8.400999999999992696 ) ) ;
#6186 = DIRECTION ( 'NONE',  ( -1.000000000000000000, -8.881784197001244435E-16, 0.000000000000000000 ) ) ;
#6187 = ORIENTED_EDGE ( 'NONE', *, *, #7344, .T. ) ;
#6188 = CIRCLE ( 'NONE', #5778, 4.250000000000008882 ) ;
#6189 = EDGE_LOOP ( 'NONE', ( #5750, #5254, #3862, #3592, #8584 ) ) ;
#6190 = CARTESIAN_POINT ( 'NONE',  ( 4.000000000000003553, -1.759474945355333109, 3.047500000000091802 ) ) ;
#6191 = ADVANCED_FACE ( 'NONE', ( #767 ), #1827, .T. ) ;
#6192 = CARTESIAN_POINT ( 'NONE',  ( 7.999999999999674039, -4.618802153517231446, -7.685468820183672278 ) ) ;
#6193 = VECTOR ( 'NONE', #4647, 1000.000000000000000 ) ;
#6194 = CARTESIAN_POINT ( 'NONE',  ( 2.309976723937096743, -7.903938623646888928, -0.1306530452037402423 ) ) ;
#6195 = PLANE ( 'NONE',  #308 ) ;
#6196 = CARTESIAN_POINT ( 'NONE',  ( -7.347286611336940609, -4.995646404165698939, -7.903039949738148273 ) ) ;
#6197 = CARTESIAN_POINT ( 'NONE',  ( -54.49999999999943157, 152.5000000000003126, 9.999999999999786837 ) ) ;
#6198 = VERTEX_POINT ( 'NONE', #6379 ) ;
#6199 = CARTESIAN_POINT ( 'NONE',  ( -32.49999999999997158, 3.469446951953614189E-15, 18.00000000000000355 ) ) ;
#6200 = EDGE_LOOP ( 'NONE', ( #3639, #2632, #7173, #6299 ) ) ;
#6201 = EDGE_CURVE ( 'NONE', #748, #7562, #5696, .T. ) ;
#6202 = DIRECTION ( 'NONE',  ( 8.659560562354899578E-17, -0.7071067811865503483, 0.7071067811865446862 ) ) ;
#6203 = DIRECTION ( 'NONE',  ( 1.000000000000000000, -0.000000000000000000, -6.938893903907228378E-17 ) ) ;
#6204 = CARTESIAN_POINT ( 'NONE',  ( 8.000000000000117240, -1.110223024625156540E-13, 0.000000000000000000 ) ) ;
#6205 = LINE ( 'NONE', #4834, #4648 ) ;
#6206 = ORIENTED_EDGE ( 'NONE', *, *, #1342, .T. ) ;
#6207 = DIRECTION ( 'NONE',  ( -1.000000000000000000, 0.000000000000000000, -6.938893903907228378E-17 ) ) ;
#6208 = VERTEX_POINT ( 'NONE', #8371 ) ;
#6209 = ORIENTED_EDGE ( 'NONE', *, *, #875, .T. ) ;
#6210 = ORIENTED_EDGE ( 'NONE', *, *, #6829, .F. ) ;
#6211 = ADVANCED_FACE ( 'NONE', ( #7025, #95, #263 ), #6297, .F. ) ;
#6212 = CARTESIAN_POINT ( 'NONE',  ( 44.99999999999992895, -425.0000000000000000, -25.00000000000001066 ) ) ;
#6213 = CARTESIAN_POINT ( 'NONE',  ( 8.000000000000012434, -1.555946510856605292, -8.332911297836602671 ) ) ;
#6214 = ORIENTED_EDGE ( 'NONE', *, *, #6370, .F. ) ;
#6215 = APPLICATION_CONTEXT ( 'automotive_design' ) ;
#6216 = CARTESIAN_POINT ( 'NONE',  ( -0.6527133886629282733, 8.860760056385709404, -7.903039949738286829 ) ) ;
#6217 = CARTESIAN_POINT ( 'NONE',  ( 275.0000000000000000, -425.0000000000000000, -75.00000000000000000 ) ) ;
#6218 = CARTESIAN_POINT ( 'NONE',  ( -350.0000000000000568, -5.551115123125782702E-14, -60.69999999999999574 ) ) ;
#6219 = EDGE_LOOP ( 'NONE', ( #1123, #5292, #6121, #1367 ) ) ;
#6220 = DIRECTION ( 'NONE',  ( 0.000000000000000000, 0.000000000000000000, 1.000000000000000000 ) ) ;
#6221 = VERTEX_POINT ( 'NONE', #8087 ) ;
#6222 = DIRECTION ( 'NONE',  ( -0.5000000000000041078, 0.8660254037844363761, 0.000000000000000000 ) ) ;
#6223 = CARTESIAN_POINT ( 'NONE',  ( 0.000000000000000000, 0.000000000000000000, -8.400000000000018119 ) ) ;
#6224 = ORIENTED_EDGE ( 'NONE', *, *, #296, .T. ) ;
#6225 = CARTESIAN_POINT ( 'NONE',  ( 0.000000000000000000, 32.50000000000005684, 18.00000000000000355 ) ) ;
#6226 = EDGE_CURVE ( 'NONE', #902, #5809, #1012, .T. ) ;
#6227 = PRODUCT_RELATED_PRODUCT_CATEGORY ( 'part', '', ( #5218 ) ) ;
#6228 = CARTESIAN_POINT ( 'NONE',  ( -8.000000000000673239, 1.572549600175905171, -0.06894455525554724074 ) ) ;
#6229 = EDGE_LOOP ( 'NONE', ( #1037, #4049, #4445, #5003 ) ) ;
#6230 = VERTEX_POINT ( 'NONE', #5650 ) ;
#6231 = DIRECTION ( 'NONE',  ( 1.774937036747276212E-30, -0.5000000000000009992, -0.8660254037844380415 ) ) ;
#6232 = DIRECTION ( 'NONE',  ( -0.9237280213470678847, -0.3830490080632384942, 0.000000000000000000 ) ) ;
#6233 = DIRECTION ( 'NONE',  ( 0.000000000000000000, 0.000000000000000000, 1.000000000000000000 ) ) ;
#6234 = ADVANCED_FACE ( 'NONE', ( #2311 ), #4967, .T. ) ;
#6235 = VECTOR ( 'NONE', #7599, 1000.000000000000000 ) ;
#6236 = FACE_OUTER_BOUND ( 'NONE', #6822, .T. ) ;
#6237 = ORIENTED_EDGE ( 'NONE', *, *, #2607, .T. ) ;
#6238 = AXIS2_PLACEMENT_3D ( 'NONE', #3517, #777, #3566 ) ;
#6239 = CARTESIAN_POINT ( 'NONE',  ( 8.000000000000015987, -3.098204225878038010, -0.3157906771918544409 ) ) ;
#6240 = ORIENTED_EDGE ( 'NONE', *, *, #4995, .F. ) ;
#6241 = DIRECTION ( 'NONE',  ( -0.000000000000000000, -0.000000000000000000, 1.000000000000000000 ) ) ;
#6242 = FACE_OUTER_BOUND ( 'NONE', #4547, .T. ) ;
#6243 = ORIENTED_EDGE ( 'NONE', *, *, #8572, .F. ) ;
#6244 = CARTESIAN_POINT ( 'NONE',  ( 0.000000000000000000, -4.685197434473812983, 0.000000000000000000 ) ) ;
#6245 = VERTEX_POINT ( 'NONE', #360 ) ;
#6246 = EDGE_CURVE ( 'NONE', #2608, #2278, #5589, .T. ) ;
#6247 = ORIENTED_EDGE ( 'NONE', *, *, #7924, .F. ) ;
#6248 = AXIS2_PLACEMENT_3D ( 'NONE', #2937, #5612, #6181 ) ;
#6249 = DIRECTION ( 'NONE',  ( 0.000000000000000000, 0.000000000000000000, -1.000000000000000000 ) ) ;
#6250 = DIRECTION ( 'NONE',  ( 1.000000000000000000, 0.000000000000000000, 0.000000000000000000 ) ) ;
#6251 = EDGE_CURVE ( 'NONE', #8125, #7090, #4485, .T. ) ;
#6252 = CARTESIAN_POINT ( 'NONE',  ( 0.000000000000000000, 0.000000000000000000, -8.400000000000018119 ) ) ;
#6253 = EDGE_LOOP ( 'NONE', ( #8338, #6793, #3999, #3323 ) ) ;
#6254 = ADVANCED_FACE ( 'NONE', ( #6453 ), #12, .T. ) ;
#6255 = DIRECTION ( 'NONE',  ( 1.000000000000000000, 0.000000000000000000, 0.000000000000000000 ) ) ;
#6256 = CYLINDRICAL_SURFACE ( 'NONE', #4164, 4.250000000000008882 ) ;
#6257 = CARTESIAN_POINT ( 'NONE',  ( 454.9999999999999432, -2.500000000001584510, 67.99999999999991473 ) ) ;
#6258 = ORIENTED_EDGE ( 'NONE', *, *, #6725, .F. ) ;
#6259 = CARTESIAN_POINT ( 'NONE',  ( 0.000000000000000000, 60.00000000000000000, -50.00000000000000000 ) ) ;
#6260 = VERTEX_POINT ( 'NONE', #7063 ) ;
#6261 = DIRECTION ( 'NONE',  ( -1.000000000000000000, 1.774937036747276562E-30, 0.000000000000000000 ) ) ;
#6262 = CIRCLE ( 'NONE', #2486, 5.500000000000023981 ) ;
#6263 = DIRECTION ( 'NONE',  ( -0.8660254037844365982, 0.5000000000000035527, -0.000000000000000000 ) ) ;
#6264 = EDGE_LOOP ( 'NONE', ( #6072, #5914 ) ) ;
#6265 = CARTESIAN_POINT ( 'NONE',  ( 6.689127551061961441, 5.375634714784386148, -0.3173508448885462019 ) ) ;
#6266 = VECTOR ( 'NONE', #7601, 1000.000000000000000 ) ;
#6267 = ORIENTED_EDGE ( 'NONE', *, *, #3487, .T. ) ;
#6268 = AXIS2_PLACEMENT_3D ( 'NONE', #6217, #6173, #8162 ) ;
#6269 = VERTEX_POINT ( 'NONE', #8534 ) ;
#6270 = DIRECTION ( 'NONE',  ( -1.000000000000000000, -2.715219353702832714E-15, 0.000000000000000000 ) ) ;
#6271 = VECTOR ( 'NONE', #4126, 1000.000000000000000 ) ;
#6272 = ADVANCED_FACE ( 'NONE', ( #4406 ), #5912, .F. ) ;
#6273 = AXIS2_PLACEMENT_3D ( 'NONE', #895, #7033, #6345 ) ;
#6274 = LINE ( 'NONE', #2251, #1639 ) ;
#6275 = VECTOR ( 'NONE', #8259, 1000.000000000000227 ) ;
#6276 = DIRECTION ( 'NONE',  ( 3.549874073494553124E-30, -1.000000000000000000, 8.626909098572831859E-16 ) ) ;
#6277 = DIRECTION ( 'NONE',  ( 1.774937036747276913E-30, -0.5000000000000014433, -0.8660254037844379305 ) ) ;
#6278 = CIRCLE ( 'NONE', #2500, 5.500000000000000000 ) ;
#6279 = FACE_OUTER_BOUND ( 'NONE', #4231, .T. ) ;
#6280 = VECTOR ( 'NONE', #886, 1000.000000000000000 ) ;
#6281 = DIRECTION ( 'NONE',  ( 0.000000000000000000, 1.078520768856843950E-29, -1.000000000000000000 ) ) ;
#6282 = ORIENTED_EDGE ( 'NONE', *, *, #5764, .F. ) ;
#6283 = COLOUR_RGB ( '',0.7921568627450980005, 0.8196078431372548767, 0.9333333333333333481 ) ;
#6284 = CIRCLE ( 'NONE', #280, 8.000000000000007105 ) ;
#6285 = CARTESIAN_POINT ( 'NONE',  ( 0.6527133886625527959, -8.860760056386080663, -0.4969600502619245797 ) ) ;
#6286 = EDGE_LOOP ( 'NONE', ( #7289, #807, #3441, #4487 ) ) ;
#6287 = AXIS2_PLACEMENT_3D ( 'NONE', #1469, #6104, #101 ) ;
#6288 = ADVANCED_FACE ( 'NONE', ( #5952 ), #8517, .T. ) ;
#6289 = CARTESIAN_POINT ( 'NONE',  ( -19.99999999999982947, 15.00000000000012434, 10.00000000000000888 ) ) ;
#6290 = VERTEX_POINT ( 'NONE', #7234 ) ;
#6291 = CARTESIAN_POINT ( 'NONE',  ( -6.686525924293513334, 5.377136764700441773, -8.083279549039747991 ) ) ;
#6292 = ORIENTED_EDGE ( 'NONE', *, *, #8231, .T. ) ;
#6293 = ORIENTED_EDGE ( 'NONE', *, *, #2683, .F. ) ;
#6294 = EDGE_CURVE ( 'NONE', #4229, #7037, #3093, .T. ) ;
#6295 = DIRECTION ( 'NONE',  ( 0.000000000000000000, 0.000000000000000000, 1.000000000000000000 ) ) ;
#6296 = B_SPLINE_CURVE_WITH_KNOTS ( 'NONE', 3,
 ( #4513, #1813, #7130, #1159, #3249, #3819 ),
 .UNSPECIFIED., .F., .F.,
 ( 4, 2, 4 ),
 ( 2.380731632781927508E-07, 0.002336973833158027380, 0.004673709593152776745 ),
 .UNSPECIFIED. ) ;
#6297 = PLANE ( 'NONE',  #6712 ) ;
#6298 = DIRECTION ( 'NONE',  ( 6.400024471206996205E-36, -1.000000000000000000, -7.598173571352216173E-18 ) ) ;
#6299 = ORIENTED_EDGE ( 'NONE', *, *, #5493, .T. ) ;
#6300 = DIRECTION ( 'NONE',  ( 1.000000000000000000, 8.881784197001244435E-16, 0.000000000000000000 ) ) ;
#6301 = CARTESIAN_POINT ( 'NONE',  ( 0.000000000000000000, -299.9999999999999432, -2.775557561562891351E-14 ) ) ;
#6302 = DIRECTION ( 'NONE',  ( 1.058471975245258048E-16, -8.736544766236844851E-16, 1.000000000000000000 ) ) ;
#6303 = VERTEX_POINT ( 'NONE', #8493 ) ;
#6304 = CARTESIAN_POINT ( 'NONE',  ( 4.000000000000003553, -3.518949890710769690, 0.000000000000000000 ) ) ;
#6305 = ORIENTED_EDGE ( 'NONE', *, *, #2083, .F. ) ;
#6306 = PLANE ( 'NONE',  #5331 ) ;
#6307 = EDGE_CURVE ( 'NONE', #8239, #2597, #3930, .T. ) ;
#6308 = PLANE ( 'NONE',  #4577 ) ;
#6309 = ORIENTED_EDGE ( 'NONE', *, *, #559, .T. ) ;
#6310 = DIRECTION ( 'NONE',  ( -0.000000000000000000, -0.000000000000000000, 1.000000000000000000 ) ) ;
#6311 = CIRCLE ( 'NONE', #4484, 8.000000000000007105 ) ;
#6312 =( LENGTH_UNIT ( ) NAMED_UNIT ( * ) SI_UNIT ( .MILLI., .METRE. ) );
#6313 = ORIENTED_EDGE ( 'NONE', *, *, #208, .F. ) ;
#6314 = EDGE_CURVE ( 'NONE', #3196, #2641, #2406, .T. ) ;
#6315 = VECTOR ( 'NONE', #700, 1000.000000000000000 ) ;
#6316 = ORIENTED_EDGE ( 'NONE', *, *, #7775, .F. ) ;
#6317 = CARTESIAN_POINT ( 'NONE',  ( 0.000000000000000000, 0.000000000000000000, 0.000000000000000000 ) ) ;
#6318 = FACE_BOUND ( 'NONE', #1677, .T. ) ;
#6319 = CIRCLE ( 'NONE', #326, 7.000000000000000888 ) ;
#6320 = DIRECTION ( 'NONE',  ( -1.000000000000000000, 0.000000000000000000, 0.000000000000000000 ) ) ;
#6321 = DIRECTION ( 'NONE',  ( -1.000000000000000000, 1.774937036747276562E-30, 0.000000000000000000 ) ) ;
#6322 = DIRECTION ( 'NONE',  ( -1.000000000000000000, 0.000000000000000000, 0.000000000000000000 ) ) ;
#6323 = LINE ( 'NONE', #7658, #3129 ) ;
#6324 = CARTESIAN_POINT ( 'NONE',  ( -39.75000000000007105, 5.103997738962193686E-34, 18.00000000000000355 ) ) ;
#6325 = ORIENTED_EDGE ( 'NONE', *, *, #8332, .F. ) ;
#6326 = CARTESIAN_POINT ( 'NONE',  ( 50.00000000000004263, 500.0000000000000000, 50.00000000000000000 ) ) ;
#6327 = ORIENTED_EDGE ( 'NONE', *, *, #1294, .F. ) ;
#6328 = CIRCLE ( 'NONE', #5911, 7.000000000000000888 ) ;
#6329 = B_SPLINE_CURVE_WITH_KNOTS ( 'NONE', 3,
 ( #375, #3805, #3022, #3686, #417, #1708 ),
 .UNSPECIFIED., .F., .F.,
 ( 4, 2, 4 ),
 ( 0.01291313371729446192, 0.01525081363757301717, 0.01758849355785157068 ),
 .UNSPECIFIED. ) ;
#6330 = VECTOR ( 'NONE', #8553, 1000.000000000000000 ) ;
#6331 = DIRECTION ( 'NONE',  ( 1.000000000000000000, 0.000000000000000000, 0.000000000000000000 ) ) ;
#6332 = CARTESIAN_POINT ( 'NONE',  ( 0.000000000000000000, -32.50000000000004974, 18.00000000000000355 ) ) ;
#6333 = ORIENTED_EDGE ( 'NONE', *, *, #1321, .F. ) ;
#6334 = ADVANCED_FACE ( 'NONE', ( #6416 ), #4077, .F. ) ;
#6335 = DIRECTION ( 'NONE',  ( -3.851859888774471706E-33, -1.232595164407830946E-32, -1.000000000000000000 ) ) ;
#6336 = CIRCLE ( 'NONE', #2569, 10.00000000000000178 ) ;
#6337 = CARTESIAN_POINT ( 'NONE',  ( -2.309976723938477416, 7.903938623647078998, -0.1306530452040687018 ) ) ;
#6338 = LINE ( 'NONE', #361, #8060 ) ;
#6339 = VERTEX_POINT ( 'NONE', #5783 ) ;
#6340 = CARTESIAN_POINT ( 'NONE',  ( 0.000000000000000000, 0.000000000000000000, 0.000000000000000000 ) ) ;
#6341 = EDGE_CURVE ( 'NONE', #1337, #1716, #8416, .T. ) ;
#6342 = CARTESIAN_POINT ( 'NONE',  ( 7.999999999999674039, -4.618802153517231446, -0.7145311798163467287 ) ) ;
#6343 = DIRECTION ( 'NONE',  ( -4.579669976578766785E-16, -5.898059818321121934E-17, -1.000000000000000000 ) ) ;
#6344 = ORIENTED_EDGE ( 'NONE', *, *, #6617, .T. ) ;
#6345 = DIRECTION ( 'NONE',  ( -0.9237280213470678847, -0.3830490080632384942, 0.000000000000000000 ) ) ;
#6346 = ORIENTED_EDGE ( 'NONE', *, *, #1254, .T. ) ;
#6347 = CARTESIAN_POINT ( 'NONE',  ( 139.1719999999995423, 3.469446951953633753E-14, -1.443289932012703503E-12 ) ) ;
#6348 = CARTESIAN_POINT ( 'NONE',  ( 5.000000000000004441, 3.513898075855358627, 2.028750000000023590 ) ) ;
#6349 = ORIENTED_EDGE ( 'NONE', *, *, #5052, .F. ) ;
#6350 = B_SPLINE_CURVE_WITH_KNOTS ( 'NONE', 3,
 ( #2196, #314, #2976, #5603, #1577, #4768 ),
 .UNSPECIFIED., .F., .F.,
 ( 4, 2, 4 ),
 ( 0.01291313371729487305, 0.01525081363757324442, 0.01758849355785161578 ),
 .UNSPECIFIED. ) ;
#6351 = CARTESIAN_POINT ( 'NONE',  ( 5.000000000000115463, 7.027796151710889561, -4.057500000000047180 ) ) ;
#6352 = ADVANCED_FACE ( 'NONE', ( #4443 ), #491, .T. ) ;
#6353 = AXIS2_PLACEMENT_3D ( 'NONE', #4747, #7961, #7912 ) ;
#6354 = EDGE_LOOP ( 'NONE', ( #214, #8221, #5536 ) ) ;
#6355 = CARTESIAN_POINT ( 'NONE',  ( 0.000000000000000000, 0.000000000000000000, 18.00000000000000355 ) ) ;
#6356 = ORIENTED_EDGE ( 'NONE', *, *, #6051, .T. ) ;
#6357 = VERTEX_POINT ( 'NONE', #2576 ) ;
#6358 = CARTESIAN_POINT ( 'NONE',  ( 4.000000000000003553, -3.518949890710769690, 0.000000000000000000 ) ) ;
#6359 = ADVANCED_BREP_SHAPE_REPRESENTATION ( '', ( #5864, #7563 ), #2282 ) ;
#6360 = DIRECTION ( 'NONE',  ( 0.000000000000000000, 0.000000000000000000, -1.000000000000000000 ) ) ;
#6361 = CARTESIAN_POINT ( 'NONE',  ( -9.999999999999888090, -14.99999999999990052, -20.00000000000001776 ) ) ;
#6362 = FACE_OUTER_BOUND ( 'NONE', #4117, .T. ) ;
#6363 = CARTESIAN_POINT ( 'NONE',  ( 8.000000000000007105, 4.618802153516732290, -8.400000000000018119 ) ) ;
#6364 = CARTESIAN_POINT ( 'NONE',  ( -1.313474075707481425, -8.479269695850799593, -0.3167204509598293694 ) ) ;
#6365 = ADVANCED_FACE ( 'NONE', ( #3137 ), #6488, .T. ) ;
#6366 = DIRECTION ( 'NONE',  ( -1.000000000000000000, 1.774937036747276562E-30, 0.000000000000000000 ) ) ;
#6367 = ORIENTED_EDGE ( 'NONE', *, *, #7413, .F. ) ;
#6368 = CARTESIAN_POINT ( 'NONE',  ( 0.000000000000000000, 0.000000000000000000, 18.00000000000000355 ) ) ;
#6369 = ORIENTED_EDGE ( 'NONE', *, *, #8279, .T. ) ;
#6370 = EDGE_CURVE ( 'NONE', #6175, #2762, #1824, .T. ) ;
#6371 = DIRECTION ( 'NONE',  ( 0.000000000000000000, 0.000000000000000000, -1.000000000000000000 ) ) ;
#6372 = CONICAL_SURFACE ( 'NONE', #1482, 8.000000000000007105, 1.047197551196597631 ) ;
#6373 = ITEM_DEFINED_TRANSFORMATION ( 'NONE', 'NONE', #7708,  #7563 ) ;
#6374 = CARTESIAN_POINT ( 'NONE',  ( 8.000000000000229150, -1.665334536937734811E-13, 0.000000000000000000 ) ) ;
#6375 = VERTEX_POINT ( 'NONE', #1174 ) ;
#6376 = CIRCLE ( 'NONE', #2877, 75.00000000000005684 ) ;
#6377 = VERTEX_POINT ( 'NONE', #525 ) ;
#6378 = DIRECTION ( 'NONE',  ( 0.000000000000000000, 0.000000000000000000, -1.000000000000000000 ) ) ;
#6379 = CARTESIAN_POINT ( 'NONE',  ( -21.99999999999958433, 120.0000000000003126, -1.763843680267613651E-29 ) ) ;
#6380 = CARTESIAN_POINT ( 'NONE',  ( 8.000000000000117240, -1.110223024625156540E-13, 0.000000000000000000 ) ) ;
#6381 = VERTEX_POINT ( 'NONE', #567 ) ;
#6382 = FACE_OUTER_BOUND ( 'NONE', #785, .T. ) ;
#6383 = FACE_OUTER_BOUND ( 'NONE', #1941, .T. ) ;
#6384 = VECTOR ( 'NONE', #3621, 1000.000000000000000 ) ;
#6385 = DIRECTION ( 'NONE',  ( -1.000000000000000000, -0.000000000000000000, -0.000000000000000000 ) ) ;
#6386 = EDGE_CURVE ( 'NONE', #5093, #5902, #3180, .T. ) ;
#6387 = CARTESIAN_POINT ( 'NONE',  ( 4.000000000000003553, -6.928203230275542523, 0.000000000000000000 ) ) ;
#6388 = ORIENTED_EDGE ( 'NONE', *, *, #1480, .T. ) ;
#6389 = DIRECTION ( 'NONE',  ( 0.000000000000000000, 5.322451846059955323E-30, -1.000000000000000000 ) ) ;
#6390 =( NAMED_UNIT ( * ) PLANE_ANGLE_UNIT ( ) SI_UNIT ( $, .RADIAN. ) );
#6391 = ORIENTED_EDGE ( 'NONE', *, *, #306, .F. ) ;
#6392 = CARTESIAN_POINT ( 'NONE',  ( 5.690023276062294855, 5.952467836903953646, -8.269346954796333193 ) ) ;
#6393 = ORIENTED_EDGE ( 'NONE', *, *, #6180, .F. ) ;
#6394 = DIRECTION ( 'NONE',  ( 1.000000000000000000, -0.000000000000000000, -6.938893903907228378E-17 ) ) ;
#6395 = ADVANCED_FACE ( 'NONE', ( #7839 ), #7822, .T. ) ;
#6396 = DIRECTION ( 'NONE',  ( 0.000000000000000000, 0.000000000000000000, 1.000000000000000000 ) ) ;
#6397 = DIRECTION ( 'NONE',  ( 3.851859888774471706E-33, 1.232595164407830946E-32, 1.000000000000000000 ) ) ;
#6398 = DIRECTION ( 'NONE',  ( 0.000000000000000000, 0.000000000000000000, 1.000000000000000000 ) ) ;
#6399 = LINE ( 'NONE', #471, #171 ) ;
#6400 = CARTESIAN_POINT ( 'NONE',  ( -5.690023276062435187, -5.952467836904131282, -8.269346954796199967 ) ) ;
#6401 = DIRECTION ( 'NONE',  ( 0.000000000000000000, -1.064348848528640545E-29, 1.000000000000000000 ) ) ;
#6402 = ORIENTED_EDGE ( 'NONE', *, *, #7889, .F. ) ;
#6403 = CARTESIAN_POINT ( 'NONE',  ( -77.99999999999945999, 120.0000000000003411, 10.00000000000000888 ) ) ;
#6404 = ORIENTED_EDGE ( 'NONE', *, *, #846, .F. ) ;
#6405 = EDGE_CURVE ( 'NONE', #8505, #2011, #7007, .T. ) ;
#6406 = AXIS2_PLACEMENT_3D ( 'NONE', #2352, #7157, #5013 ) ;
#6407 = CARTESIAN_POINT ( 'NONE',  ( 8.000000000000008882, 1.572549600175701778, -8.331055444744873029 ) ) ;
#6408 = CARTESIAN_POINT ( 'NONE',  ( 8.000000000000229150, -4.440892098500626162E-13, -8.400000000000018119 ) ) ;
#6409 = ORIENTED_EDGE ( 'NONE', *, *, #1759, .F. ) ;
#6410 = DIRECTION ( 'NONE',  ( 0.000000000000000000, 0.000000000000000000, 1.000000000000000000 ) ) ;
#6411 = VECTOR ( 'NONE', #1022, 1000.000000000000000 ) ;
#6412 = AXIS2_PLACEMENT_3D ( 'NONE', #1945, #595, #3743 ) ;
#6413 = ADVANCED_FACE ( 'NONE', ( #7977 ), #3406, .T. ) ;
#6414 = PLANE ( 'NONE',  #4646 ) ;
#6415 = EDGE_CURVE ( 'NONE', #4181, #7660, #3451, .T. ) ;
#6416 = FACE_OUTER_BOUND ( 'NONE', #3868, .T. ) ;
#6417 = DIRECTION ( 'NONE',  ( -1.463706757734299248E-32, 1.000000000000000000, 5.238529448733281520E-32 ) ) ;
#6418 = EDGE_LOOP ( 'NONE', ( #4416, #2125, #1305 ) ) ;
#6419 = CARTESIAN_POINT ( 'NONE',  ( 10.00000000000000888, 0.000000000000000000, 4.440892098500626162E-13 ) ) ;
#6420 = DIRECTION ( 'NONE',  ( -0.000000000000000000, -0.000000000000000000, 1.000000000000000000 ) ) ;
#6421 = AXIS2_PLACEMENT_3D ( 'NONE', #8289, #4970, #4368 ) ;
#6422 = DIRECTION ( 'NONE',  ( 0.000000000000000000, -4.930380657631255821E-30, 1.000000000000000000 ) ) ;
#6423 = LINE ( 'NONE', #7683, #4871 ) ;
#6424 = ORIENTED_EDGE ( 'NONE', *, *, #3242, .F. ) ;
#6425 = DIRECTION ( 'NONE',  ( 1.000000000000000000, -1.774937036747276562E-30, -9.447016907875728896E-60 ) ) ;
#6426 = VERTEX_POINT ( 'NONE', #7459 ) ;
#6427 = EDGE_CURVE ( 'NONE', #1200, #3003, #6041, .T. ) ;
#6428 = CARTESIAN_POINT ( 'NONE',  ( 2.645508037661670642, 7.710219529346487910, -8.331901280394694354 ) ) ;
#6429 = ORIENTED_EDGE ( 'NONE', *, *, #5786, .T. ) ;
#6430 = CARTESIAN_POINT ( 'NONE',  ( 1.313474075707311117, 8.479269695850856436, -8.083279549040174317 ) ) ;
#6431 = VECTOR ( 'NONE', #7487, 1000.000000000000000 ) ;
#6432 = LINE ( 'NONE', #6361, #1748 ) ;
#6433 = CARTESIAN_POINT ( 'NONE',  ( -44.99999999999992895, 425.0000000000000000, -25.00000000000000355 ) ) ;
#6434 = AXIS2_PLACEMENT_3D ( 'NONE', #1212, #5985, #654 ) ;
#6435 = CARTESIAN_POINT ( 'NONE',  ( 0.000000000000000000, 299.9999999999999432, -6.938893903907228378E-14 ) ) ;
#6436 = CARTESIAN_POINT ( 'NONE',  ( 32.30950000000065359, 0.000000000000000000, 6.883382752675970551E-12 ) ) ;
#6437 = CARTESIAN_POINT ( 'NONE',  ( -4.250000000000000888, -32.50000000000004974, 18.00000000000000355 ) ) ;
#6438 = DIRECTION ( 'NONE',  ( 0.000000000000000000, 0.000000000000000000, 1.000000000000000000 ) ) ;
#6439 = VERTEX_POINT ( 'NONE', #7359 ) ;
#6440 = AXIS2_PLACEMENT_3D ( 'NONE', #8208, #5426, #2853 ) ;
#6441 = EDGE_CURVE ( 'NONE', #4775, #4975, #1700, .T. ) ;
#6442 = ORIENTED_EDGE ( 'NONE', *, *, #6307, .T. ) ;
#6443 = AXIS2_PLACEMENT_3D ( 'NONE', #4175, #163, #8105 ) ;
#6444 = DIRECTION ( 'NONE',  ( 0.000000000000000000, 0.000000000000000000, 1.000000000000000000 ) ) ;
#6445 = CARTESIAN_POINT ( 'NONE',  ( 0.000000000000000000, 0.000000000000000000, 0.000000000000000000 ) ) ;
#6446 = ORIENTED_EDGE ( 'NONE', *, *, #2756, .F. ) ;
#6447 = EDGE_LOOP ( 'NONE', ( #5468, #3166 ) ) ;
#6448 = EDGE_CURVE ( 'NONE', #173, #927, #22, .T. ) ;
#6449 = VECTOR ( 'NONE', #2925, 1000.000000000000000 ) ;
#6450 = ADVANCED_BREP_SHAPE_REPRESENTATION ( '', ( #5753, #7563 ), #4234 ) ;
#6451 = DIRECTION ( 'NONE',  ( -0.9237280213470678847, -0.3830490080632384942, 0.000000000000000000 ) ) ;
#6452 = DIRECTION ( 'NONE',  ( 1.000000000000000000, 2.715219353702832714E-15, 0.000000000000000000 ) ) ;
#6453 = FACE_OUTER_BOUND ( 'NONE', #6811, .T. ) ;
#6454 = CARTESIAN_POINT ( 'NONE',  ( 5.355005115540882876, 6.145890662064627641, -0.08224679563969784779 ) ) ;
#6455 = ORIENTED_EDGE ( 'NONE', *, *, #4427, .F. ) ;
#6456 = CARTESIAN_POINT ( 'NONE',  ( 4.000000000000003553, 1.759474945355374409, 3.047499999999869758 ) ) ;
#6457 = DIRECTION ( 'NONE',  ( 1.000000000000000000, 0.000000000000000000, 0.000000000000000000 ) ) ;
#6458 = CARTESIAN_POINT ( 'NONE',  ( 5.000000000000004441, -4.163336342344337027E-14, 4.057500000000047180 ) ) ;
#6459 = CARTESIAN_POINT ( 'NONE',  ( 455.0000000000002842, 62.49999999999838707, 67.99999999999991473 ) ) ;
#6460 = DIRECTION ( 'NONE',  ( 0.000000000000000000, 0.000000000000000000, 1.000000000000000000 ) ) ;
#6461 = DIRECTION ( 'NONE',  ( 1.000000000000000000, 0.000000000000000000, 0.000000000000000000 ) ) ;
#6462 = ORIENTED_EDGE ( 'NONE', *, *, #6539, .T. ) ;
#6463 = CARTESIAN_POINT ( 'NONE',  ( 3.200012235603505854E-34, -50.00000000000008527, -10.00000000000006395 ) ) ;
#6464 = SHAPE_REPRESENTATION_RELATIONSHIP ( 'NONE' , 'NONE' ,  #4003, #841 ) ;
#6465 = EDGE_LOOP ( 'NONE', ( #2174, #275 ) ) ;
#6466 = DIRECTION ( 'NONE',  ( -1.000000000000000000, 3.549874073494553124E-30, 0.000000000000000000 ) ) ;
#6467 = ORIENTED_EDGE ( 'NONE', *, *, #424, .T. ) ;
#6468 = DIRECTION ( 'NONE',  ( -1.463706757734299248E-32, 1.000000000000000000, 5.238529448733281520E-32 ) ) ;
#6469 = DIRECTION ( 'NONE',  ( 1.000000000000000000, 3.083952846180994816E-15, 0.000000000000000000 ) ) ;
#6470 = ADVANCED_FACE ( 'NONE', ( #4624, #6162, #747 ), #6079, .T. ) ;
#6471 = AXIS2_PLACEMENT_3D ( 'NONE', #8362, #1203, #3861 ) ;
#6472 = DIRECTION ( 'NONE',  ( -3.919652622816902408E-30, -3.944304526105059027E-30, 1.000000000000000000 ) ) ;
#6473 = DIRECTION ( 'NONE',  ( 0.000000000000000000, 0.000000000000000000, -1.000000000000000000 ) ) ;
#6474 = DIRECTION ( 'NONE',  ( -0.5000000000000033307, -0.8660254037844367092, 0.000000000000000000 ) ) ;
#6475 = CARTESIAN_POINT ( 'NONE',  ( -4.440892098500626162E-13, -9.237604307034018802, -7.685468820183672278 ) ) ;
#6476 = ORIENTED_EDGE ( 'NONE', *, *, #558, .F. ) ;
#6477 = ORIENTED_EDGE ( 'NONE', *, *, #1626, .T. ) ;
#6478 = CARTESIAN_POINT ( 'NONE',  ( 275.0000000000000000, -425.0000000000000000, 0.000000000000000000 ) ) ;
#6479 = EDGE_CURVE ( 'NONE', #4142, #92, #4842, .T. ) ;
#6480 = CONTEXT_DEPENDENT_SHAPE_REPRESENTATION ( #2228, #1738 ) ;
#6481 = CARTESIAN_POINT ( 'NONE',  ( 0.6543471694407191341, 8.859816792613939285, -7.903584543331081846 ) ) ;
#6482 = ORIENTED_EDGE ( 'NONE', *, *, #8219, .F. ) ;
#6483 = FACE_OUTER_BOUND ( 'NONE', #2456, .T. ) ;
#6484 = VERTEX_POINT ( 'NONE', #77 ) ;
#6485 = AXIS2_PLACEMENT_3D ( 'NONE', #5885, #4074, #2073 ) ;
#6486 = DIRECTION ( 'NONE',  ( -1.000000000000000000, -3.083952846180997183E-15, 0.000000000000000000 ) ) ;
#6487 = EDGE_CURVE ( 'NONE', #1229, #2950, #4777, .T. ) ;
#6488 = PLANE ( 'NONE',  #5329 ) ;
#6489 = CARTESIAN_POINT ( 'NONE',  ( 50.00000000000004263, 500.0000000000000000, -45.00000000000000711 ) ) ;
#6490 = ORIENTED_EDGE ( 'NONE', *, *, #1794, .T. ) ;
#6491 = CARTESIAN_POINT ( 'NONE',  ( 8.000000000000007105, -4.618802153517121312, -8.400000000000018119 ) ) ;
#6492 = CONICAL_SURFACE ( 'NONE', #7057, 8.000000000000007105, 1.047197551196597631 ) ;
#6493 = DIRECTION ( 'NONE',  ( -1.058471975245261993E-16, 8.736544766236848795E-16, -1.000000000000000000 ) ) ;
#6494 = CONICAL_SURFACE ( 'NONE', #4412, 8.000000000000007105, 1.047197551196597631 ) ;
#6495 = EDGE_CURVE ( 'NONE', #462, #7120, #2035, .T. ) ;
#6496 = DIRECTION ( 'NONE',  ( -3.851859888774471706E-33, 7.598173571352185358E-18, -1.000000000000000000 ) ) ;
#6497 = VERTEX_POINT ( 'NONE', #7928 ) ;
#6498 = ADVANCED_FACE ( 'NONE', ( #6034 ), #6872, .T. ) ;
#6499 = CARTESIAN_POINT ( 'NONE',  ( 4.000000000000003553, -1.759474945355333109, 3.047500000000091802 ) ) ;
#6500 = PLANE ( 'NONE',  #123 ) ;
#6501 = ORIENTED_EDGE ( 'NONE', *, *, #6583, .F. ) ;
#6502 = AXIS2_PLACEMENT_3D ( 'NONE', #3466, #93, #6263 ) ;
#6503 = EDGE_CURVE ( 'NONE', #5776, #982, #5775, .T. ) ;
#6504 = DIRECTION ( 'NONE',  ( -0.5000000000000033307, -0.8660254037844367092, 0.000000000000000000 ) ) ;
#6505 = ORIENTED_EDGE ( 'NONE', *, *, #643, .T. ) ;
#6506 = CARTESIAN_POINT ( 'NONE',  ( -31.74999999999994316, -1.972152263052529514E-28, 0.000000000000000000 ) ) ;
#6507 = CARTESIAN_POINT ( 'NONE',  ( -44.99999999999992895, 500.0000000000000000, -45.00000000000000711 ) ) ;
#6508 = AXIS2_PLACEMENT_3D ( 'NONE', #2865, #1633, #6322 ) ;
#6509 = DIRECTION ( 'NONE',  ( 1.000000000000000000, 0.000000000000000000, 0.000000000000000000 ) ) ;
#6510 = CARTESIAN_POINT ( 'NONE',  ( 9.999999999999896971, 0.000000000000000000, 0.000000000000000000 ) ) ;
#6511 = CARTESIAN_POINT ( 'NONE',  ( 50.00000000000004263, 500.0000000000000000, 50.00000000000000000 ) ) ;
#6512 = FACE_OUTER_BOUND ( 'NONE', #311, .T. ) ;
#6513 = ORIENTED_EDGE ( 'NONE', *, *, #6918, .F. ) ;
#6514 =( LENGTH_UNIT ( ) NAMED_UNIT ( * ) SI_UNIT ( .MILLI., .METRE. ) );
#6515 = ORIENTED_EDGE ( 'NONE', *, *, #5016, .F. ) ;
#6516 = LINE ( 'NONE', #6610, #4442 ) ;
#6517 = VECTOR ( 'NONE', #3926, 1000.000000000000000 ) ;
#6518 = CONICAL_SURFACE ( 'NONE', #2270, 8.000000000000007105, 1.047197551196597631 ) ;
#6519 = DIRECTION ( 'NONE',  ( -1.000000000000000000, -7.194245199571014382E-14, 0.000000000000000000 ) ) ;
#6520 = APPLICATION_CONTEXT ( 'automotive_design' ) ;
#6521 = ORIENTED_EDGE ( 'NONE', *, *, #7556, .F. ) ;
#6522 = LINE ( 'NONE', #7140, #8335 ) ;
#6523 = CIRCLE ( 'NONE', #693, 4.000000000000060396 ) ;
#6524 = VERTEX_POINT ( 'NONE', #2053 ) ;
#6525 = DIRECTION ( 'NONE',  ( 3.851859888774471706E-33, -7.598173571352223877E-18, 1.000000000000000000 ) ) ;
#6526 = ORIENTED_EDGE ( 'NONE', *, *, #708, .T. ) ;
#6527 = CIRCLE ( 'NONE', #6134, 4.250000000000008882 ) ;
#6528 = ADVANCED_FACE ( 'NONE', ( #7408 ), #4712, .T. ) ;
#6529 = DIRECTION ( 'NONE',  ( 0.000000000000000000, -1.213383262747659708E-29, 1.000000000000000000 ) ) ;
#6530 = ORIENTED_EDGE ( 'NONE', *, *, #2143, .T. ) ;
#6531 = AXIS2_PLACEMENT_3D ( 'NONE', #6301, #4279, #4812 ) ;
#6532 = CARTESIAN_POINT ( 'NONE',  ( 5.000000000000115463, -14.99999999999990230, -20.00000000000001776 ) ) ;
#6533 = CARTESIAN_POINT ( 'NONE',  ( 4.000000000000003553, -2.639212418033074936, 1.523750000000045901 ) ) ;
#6534 = DIRECTION ( 'NONE',  ( 1.000000000000000000, 0.000000000000000000, 0.000000000000000000 ) ) ;
#6535 = LINE ( 'NONE', #4672, #4334 ) ;
#6536 = ORIENTED_EDGE ( 'NONE', *, *, #7597, .F. ) ;
#6537 = CARTESIAN_POINT ( 'NONE',  ( 50.00000000000004263, 500.0000000000000000, -50.00000000000000000 ) ) ;
#6538 = VECTOR ( 'NONE', #7072, 1000.000000000000000 ) ;
#6539 = EDGE_CURVE ( 'NONE', #3768, #6303, #6768, .T. ) ;
#6540 = CONTEXT_DEPENDENT_SHAPE_REPRESENTATION ( #411, #2798 ) ;
#6541 = ADVANCED_FACE ( 'NONE', ( #8151 ), #3535, .T. ) ;
#6542 = DIRECTION ( 'NONE',  ( -0.000000000000000000, -0.000000000000000000, 1.000000000000000000 ) ) ;
#6543 = VERTEX_POINT ( 'NONE', #6374 ) ;
#6544 = DIRECTION ( 'NONE',  ( 1.774937036747276913E-30, -0.5000000000000014433, -0.8660254037844379305 ) ) ;
#6545 = CARTESIAN_POINT ( 'NONE',  ( 0.000000000000000000, 9.237604307034130713, -8.400000000000018119 ) ) ;
#6546 = VERTEX_POINT ( 'NONE', #215 ) ;
#6547 = ADVANCED_FACE ( 'NONE', ( #4999 ), #5275, .T. ) ;
#6548 = CYLINDRICAL_SURFACE ( 'NONE', #2396, 5.559999999999998721 ) ;
#6549 = ORIENTED_EDGE ( 'NONE', *, *, #4884, .F. ) ;
#6550 = CARTESIAN_POINT ( 'NONE',  ( 8.000000000000117240, 4.618802153517009401, -7.685468820183672278 ) ) ;
#6551 = PRODUCT_DEFINITION_CONTEXT ( 'detailed design', #3030, 'design' ) ;
#6552 = B_SPLINE_CURVE_WITH_KNOTS ( 'NONE', 3,
 ( #2563, #395, #6407, #8441, #5119, #1864 ),
 .UNSPECIFIED., .F., .F.,
 ( 4, 2, 4 ),
 ( 0.01291313371729433702, 0.01525081363757292696, 0.01758849355785151516 ),
 .UNSPECIFIED. ) ;
#6553 = CARTESIAN_POINT ( 'NONE',  ( 1.137165254206398273E-13, -414.9999999999999432, -19.50000000000003197 ) ) ;
#6554 = DIRECTION ( 'NONE',  ( -1.463706757734299248E-32, 1.000000000000000000, 5.238529448733281520E-32 ) ) ;
#6555 = DIRECTION ( 'NONE',  ( -1.000000000000000000, -4.440892098500625373E-15, 0.000000000000000000 ) ) ;
#6556 = CARTESIAN_POINT ( 'NONE',  ( -8.000000000000117240, -1.110223024625156540E-13, -8.400000000000018119 ) ) ;
#6557 = ORIENTED_EDGE ( 'NONE', *, *, #3292, .T. ) ;
#6558 = ORIENTED_EDGE ( 'NONE', *, *, #2194, .T. ) ;
#6559 = DIRECTION ( 'NONE',  ( -1.000000000000000000, -8.881784197001244435E-16, 0.000000000000000000 ) ) ;
#6560 = ADVANCED_FACE ( 'NONE', ( #2304 ), #301, .T. ) ;
#6561 = CIRCLE ( 'NONE', #7958, 4.499999999999983125 ) ;
#6562 = CARTESIAN_POINT ( 'NONE',  ( -8.000000000000222045, -3.098204225878420814, -0.3157906771920435673 ) ) ;
#6563 = AXIS2_PLACEMENT_3D ( 'NONE', #1982, #8508, #544 ) ;
#6564 = VECTOR ( 'NONE', #5621, 1000.000000000000000 ) ;
#6565 = CARTESIAN_POINT ( 'NONE',  ( -6.686525924292766376, 5.377136764700066074, -0.3167204509597931761 ) ) ;
#6566 = EDGE_LOOP ( 'NONE', ( #1658, #1800, #8451, #6349 ) ) ;
#6567 = AXIS2_PLACEMENT_3D ( 'NONE', #5839, #1109, #3773 ) ;
#6568 = EDGE_CURVE ( 'NONE', #8133, #5078, #2235, .T. ) ;
#6569 = EDGE_CURVE ( 'NONE', #6850, #2145, #8197, .T. ) ;
#6570 = DIRECTION ( 'NONE',  ( 0.000000000000000000, 0.000000000000000000, -1.000000000000000000 ) ) ;
#6571 = ORIENTED_EDGE ( 'NONE', *, *, #2386, .F. ) ;
#6572 = ORIENTED_EDGE ( 'NONE', *, *, #2155, .T. ) ;
#6573 = AXIS2_PLACEMENT_3D ( 'NONE', #6456, #1264, #2483 ) ;
#6574 = FACE_OUTER_BOUND ( 'NONE', #5403, .T. ) ;
#6575 = ORIENTED_EDGE ( 'NONE', *, *, #7969, .T. ) ;
#6576 = CONICAL_SURFACE ( 'NONE', #3664, 8.000000000000007105, 1.047197551196597631 ) ;
#6577 = CARTESIAN_POINT ( 'NONE',  ( 0.000000000000000000, -294.9999999999998295, -2.775557561562891351E-14 ) ) ;
#6578 = CARTESIAN_POINT ( 'NONE',  ( 8.000000000000119016, 3.115336682266876434, -0.3193931313915404635 ) ) ;
#6579 = DIRECTION ( 'NONE',  ( -3.549874073494553124E-30, 1.000000000000000000, -8.626909098572831859E-16 ) ) ;
#6580 = AXIS2_PLACEMENT_3D ( 'NONE', #3223, #4140, #2668 ) ;
#6581 = AXIS2_PLACEMENT_3D ( 'NONE', #764, #3421, #809 ) ;
#6582 = DIRECTION ( 'NONE',  ( 8.659560562354956277E-17, -0.7071067811865456854, 0.7071067811865493491 ) ) ;
#6583 = EDGE_CURVE ( 'NONE', #5323, #2182, #4144, .T. ) ;
#6584 = VERTEX_POINT ( 'NONE', #6244 ) ;
#6585 = CARTESIAN_POINT ( 'NONE',  ( 5.000000000000004441, 4.685197434473897360, 0.000000000000000000 ) ) ;
#6586 = AXIS2_PLACEMENT_3D ( 'NONE', #3540, #8029, #4841 ) ;
#6587 = APPLICATION_PROTOCOL_DEFINITION ( 'draft international standard', 'automotive_design', 1998, #8581 ) ;
#6588 = AXIS2_PLACEMENT_3D ( 'NONE', #6506, #7855, #2681 ) ;
#6589 = AXIS2_PLACEMENT_3D ( 'NONE', #4428, #7089, #1121 ) ;
#6590 = CARTESIAN_POINT ( 'NONE',  ( -17.49999999999955236, 120.0000000000003268, 9.999999999999980460 ) ) ;
#6591 = EDGE_CURVE ( 'NONE', #5825, #2630, #4962, .T. ) ;
#6592 = VERTEX_POINT ( 'NONE', #7539 ) ;
#6593 = CARTESIAN_POINT ( 'NONE',  ( 8.000000000000117240, -1.110223024625156540E-13, -8.400000000000018119 ) ) ;
#6594 = CARTESIAN_POINT ( 'NONE',  ( 0.000000000000000000, 0.000000000000000000, 0.000000000000000000 ) ) ;
#6595 = EDGE_LOOP ( 'NONE', ( #4984, #3857, #4153, #4408 ) ) ;
#6596 = AXIS2_PLACEMENT_3D ( 'NONE', #8588, #2065, #2629 ) ;
#6597 = CARTESIAN_POINT ( 'NONE',  ( 0.000000000000000000, 0.000000000000000000, 18.00000000000000355 ) ) ;
#6598 = ORIENTED_EDGE ( 'NONE', *, *, #6405, .F. ) ;
#6599 = LINE ( 'NONE', #631, #1306 ) ;
#6600 = CARTESIAN_POINT ( 'NONE',  ( 3.319543390095996749, -7.321065037175506163, -8.383111142572218455 ) ) ;
#6601 = AXIS2_PLACEMENT_3D ( 'NONE', #4972, #1746, #6493 ) ;
#6602 = ADVANCED_FACE ( 'NONE', ( #1565 ), #5543, .F. ) ;
#6603 = DIRECTION ( 'NONE',  ( -1.000000000000000000, -2.715219353702832714E-15, 0.000000000000000000 ) ) ;
#6604 = DIRECTION ( 'NONE',  ( 1.000000000000000000, -1.774937036747276562E-30, -9.447016907875728896E-60 ) ) ;
#6605 = FACE_BOUND ( 'NONE', #5501, .T. ) ;
#6606 = CARTESIAN_POINT ( 'NONE',  ( 5.690023276062453839, 5.952467836904148157, -0.1306530452038311141 ) ) ;
#6607 = ORIENTED_EDGE ( 'NONE', *, *, #3879, .T. ) ;
#6608 = SURFACE_SIDE_STYLE ('',( #3431 ) ) ;
#6609 = ORIENTED_EDGE ( 'NONE', *, *, #424, .F. ) ;
#6610 = CARTESIAN_POINT ( 'NONE',  ( -8.000000000000007105, -4.618802153517398423, -8.400000000000018119 ) ) ;
#6611 = DIRECTION ( 'NONE',  ( -5.620633949699709114E-30, 0.8660254037844393737, 0.4999999999999987232 ) ) ;
#6612 = EDGE_CURVE ( 'NONE', #2931, #218, #4836, .T. ) ;
#6613 = DIRECTION ( 'NONE',  ( -1.000000000000000000, 0.000000000000000000, -6.938893903907228378E-17 ) ) ;
#6614 = CARTESIAN_POINT ( 'NONE',  ( -25.74999999999982947, 15.00000000000010836, 10.00000000000000888 ) ) ;
#6615 = PRODUCT ( 'Conveyor roller', 'Conveyor roller', '', ( #2580 ) ) ;
#6616 = CARTESIAN_POINT ( 'NONE',  ( -7.999999999999894307, 1.572549600175527917, -8.331055444744958294 ) ) ;
#6617 = EDGE_CURVE ( 'NONE', #2020, #1855, #7623, .T. ) ;
#6618 = CARTESIAN_POINT ( 'NONE',  ( 5.354491962338145505, -6.146186931204510984, -0.06809871960548105618 ) ) ;
#6619 = FACE_OUTER_BOUND ( 'NONE', #8018, .T. ) ;
#6620 = ORIENTED_EDGE ( 'NONE', *, *, #6441, .F. ) ;
#6621 = AXIS2_PLACEMENT_3D ( 'NONE', #2384, #482, #2520 ) ;
#6622 = CARTESIAN_POINT ( 'NONE',  ( 0.000000000000000000, 0.000000000000000000, 0.000000000000000000 ) ) ;
#6623 = VERTEX_POINT ( 'NONE', #5502 ) ;
#6624 = DIRECTION ( 'NONE',  ( 7.420547859534711256E-34, -1.000000000000000000, -1.224646799147352961E-16 ) ) ;
#6625 = EDGE_LOOP ( 'NONE', ( #6282, #4843, #652 ) ) ;
#6626 = CARTESIAN_POINT ( 'NONE',  ( 0.000000000000000000, 60.00000000000000000, -45.00000000000000711 ) ) ;
#6627 = EDGE_CURVE ( 'NONE', #6290, #2098, #5644, .T. ) ;
#6628 = FACE_OUTER_BOUND ( 'NONE', #3355, .T. ) ;
#6629 = CARTESIAN_POINT ( 'NONE',  ( -7.999999999999998224, -1.555946510856075493, -8.332911297836668396 ) ) ;
#6630 = VERTEX_POINT ( 'NONE', #5594 ) ;
#6631 = LINE ( 'NONE', #6491, #174 ) ;
#6632 = APPLICATION_PROTOCOL_DEFINITION ( 'draft international standard', 'automotive_design', 1998, #120 ) ;
#6633 = AXIS2_PLACEMENT_3D ( 'NONE', #720, #6058, #4601 ) ;
#6634 = CARTESIAN_POINT ( 'NONE',  ( -275.0000000000000000, 425.0000000000000000, 1.561424668912875158E-13 ) ) ;
#6635 = DIRECTION ( 'NONE',  ( 1.000000000000000000, 0.000000000000000000, 0.000000000000000000 ) ) ;
#6636 = VERTEX_POINT ( 'NONE', #1641 ) ;
#6637 = DIRECTION ( 'NONE',  ( 0.000000000000000000, 0.000000000000000000, 1.000000000000000000 ) ) ;
#6638 = AXIS2_PLACEMENT_3D ( 'NONE', #1292, #3950, #1990 ) ;
#6639 = DIRECTION ( 'NONE',  ( 1.000000000000000000, 0.000000000000000000, 0.000000000000000000 ) ) ;
#6640 = ORIENTED_EDGE ( 'NONE', *, *, #3356, .T. ) ;
#6641 = DIRECTION ( 'NONE',  ( -3.919652622816902408E-30, -3.944304526105059027E-30, 1.000000000000000000 ) ) ;
#6642 = VERTEX_POINT ( 'NONE', #7581 ) ;
#6643 = DIRECTION ( 'NONE',  ( 0.000000000000000000, 0.4999999999999983902, -0.8660254037844395958 ) ) ;
#6644 = EDGE_CURVE ( 'NONE', #5838, #5920, #2614, .T. ) ;
#6645 = APPLICATION_CONTEXT ( 'automotive_design' ) ;
#6646 = CARTESIAN_POINT ( 'NONE',  ( 1.310872448937626222, -8.480771745766677583, -8.082649155111246486 ) ) ;
#6647 = CARTESIAN_POINT ( 'NONE',  ( 0.000000000000000000, 0.000000000000000000, 16.99999999999991829 ) ) ;
#6648 = LINE ( 'NONE', #8596, #6957 ) ;
#6649 = FACE_OUTER_BOUND ( 'NONE', #6707, .T. ) ;
#6650 = AXIS2_PLACEMENT_3D ( 'NONE', #1621, #1499, #6139 ) ;
#6651 = FACE_OUTER_BOUND ( 'NONE', #1868, .T. ) ;
#6652 = ORIENTED_EDGE ( 'NONE', *, *, #2038, .T. ) ;
#6653 = CARTESIAN_POINT ( 'NONE',  ( 4.680456609904014798, 6.535341423375668590, -0.01688885742781526603 ) ) ;
#6654 = EDGE_LOOP ( 'NONE', ( #3312, #3459, #7302, #2783 ) ) ;
#6655 = DIRECTION ( 'NONE',  ( 0.000000000000000000, -1.064348848528640545E-29, 1.000000000000000000 ) ) ;
#6656 = ADVANCED_FACE ( 'NONE', ( #3710 ), #6934, .F. ) ;
#6657 = PLANE ( 'NONE',  #2740 ) ;
#6658 = CARTESIAN_POINT ( 'NONE',  ( 4.681481898396925523, -6.534749472788247360, -2.235319947804098595E-14 ) ) ;
#6659 = CARTESIAN_POINT ( 'NONE',  ( -7.999999999999896083, 4.618802153516899267, -0.7145311798163467287 ) ) ;
#6660 = ITEM_DEFINED_TRANSFORMATION ( 'NONE', 'NONE', #339,  #7563 ) ;
#6661 = DIRECTION ( 'NONE',  ( 0.000000000000000000, 0.000000000000000000, 1.000000000000000000 ) ) ;
#6662 = DIRECTION ( 'NONE',  ( 1.774937036747276562E-30, -1.000000000000000000, 1.110768649713241713E-15 ) ) ;
#6663 = ORIENTED_EDGE ( 'NONE', *, *, #4642, .F. ) ;
#6664 = CARTESIAN_POINT ( 'NONE',  ( -8.000000000000229150, 4.440892098500626162E-13, 0.000000000000000000 ) ) ;
#6665 = ORIENTED_EDGE ( 'NONE', *, *, #2119, .F. ) ;
#6666 = ADVANCED_FACE ( 'NONE', ( #3666 ), #4014, .T. ) ;
#6667 = CARTESIAN_POINT ( 'NONE',  ( -4.000000000000003553, 6.928203230275209457, 0.000000000000000000 ) ) ;
#6668 = CARTESIAN_POINT ( 'NONE',  ( 8.000000000000007105, 4.618802153516732290, -0.7145311798163467287 ) ) ;
#6669 = CIRCLE ( 'NONE', #7767, 8.000000000000007105 ) ;
#6670 = DIRECTION ( 'NONE',  ( 0.000000000000000000, 0.000000000000000000, 1.000000000000000000 ) ) ;
#6671 = B_SPLINE_CURVE_WITH_KNOTS ( 'NONE', 3,
 ( #3960, #1998, #649, #4791, #5357, #6758 ),
 .UNSPECIFIED., .F., .F.,
 ( 4, 2, 4 ),
 ( 2.380731634175168328E-07, 0.002336973833158143606, 0.004673709593152869553 ),
 .UNSPECIFIED. ) ;
#6672 = CARTESIAN_POINT ( 'NONE',  ( 1.310872448938031454, -8.480771745766503500, -0.3173508448887171207 ) ) ;
#6673 = CARTESIAN_POINT ( 'NONE',  ( -64.99999999999944578, 120.0000000000002842, 9.999999999999980460 ) ) ;
#6674 = EDGE_LOOP ( 'NONE', ( #3483, #2724 ) ) ;
#6675 = EDGE_LOOP ( 'NONE', ( #2745, #8476 ) ) ;
#6676 = EDGE_CURVE ( 'NONE', #181, #5920, #4524, .T. ) ;
#6677 = APPLICATION_PROTOCOL_DEFINITION ( 'draft international standard', 'automotive_design', 1998, #7696 ) ;
#6678 = MECHANICAL_DESIGN_GEOMETRIC_PRESENTATION_REPRESENTATION (  '', ( #3883 ), #1392 ) ;
#6679 = AXIS2_PLACEMENT_3D ( 'NONE', #6259, #272, #186 ) ;
#6680 = CIRCLE ( 'NONE', #5999, 8.000000000000007105 ) ;
#6681 = DIRECTION ( 'NONE',  ( 6.400024471207029615E-36, -1.000000000000000000, 0.000000000000000000 ) ) ;
#6682 = ORIENTED_EDGE ( 'NONE', *, *, #6764, .T. ) ;
#6683 = AXIS2_PLACEMENT_3D ( 'NONE', #6590, #1883, #5377 ) ;
#6684 = CARTESIAN_POINT ( 'NONE',  ( 8.000000000000234479, 1.572549600175502604, -8.331055444744771776 ) ) ;
#6685 = ORIENTED_EDGE ( 'NONE', *, *, #7148, .T. ) ;
#6686 = AXIS2_PLACEMENT_3D ( 'NONE', #3856, #5893, #437 ) ;
#6687 = CARTESIAN_POINT ( 'NONE',  ( 0.000000000000000000, 0.000000000000000000, 10.00000000000000888 ) ) ;
#6688 = ORIENTED_EDGE ( 'NONE', *, *, #8604, .T. ) ;
#6689 = LINE ( 'NONE', #8546, #2393 ) ;
#6690 = AXIS2_PLACEMENT_3D ( 'NONE', #2611, #4096, #5406 ) ;
#6691 = CARTESIAN_POINT ( 'NONE',  ( 5.500000000000000000, 0.000000000000000000, -50.00000000000000000 ) ) ;
#6692 = CARTESIAN_POINT ( 'NONE',  ( 15.00000000000002487, 1.836970198721033139E-15, 18.00000000000000355 ) ) ;
#6693 = CARTESIAN_POINT ( 'NONE',  ( -4.000000000000114575, -6.928203230275542523, 0.000000000000000000 ) ) ;
#6694 = DIRECTION ( 'NONE',  ( -3.919652622816902408E-30, -3.944304526105059027E-30, 1.000000000000000000 ) ) ;
#6695 = EDGE_CURVE ( 'NONE', #4476, #7908, #959, .T. ) ;
#6696 = DIRECTION ( 'NONE',  ( 1.000000000000000000, 0.000000000000000000, 0.000000000000000000 ) ) ;
#6697 = CARTESIAN_POINT ( 'NONE',  ( -7.347286611337208839, -4.995646404165207777, -0.4969600502618418680 ) ) ;
#6698 = ORIENTED_EDGE ( 'NONE', *, *, #5491, .T. ) ;
#6699 = VERTEX_POINT ( 'NONE', #2470 ) ;
#6700 = DIRECTION ( 'NONE',  ( -1.000000000000000000, -0.000000000000000000, -0.000000000000000000 ) ) ;
#6701 = FILL_AREA_STYLE ('',( #7178 ) ) ;
#6702 = DIRECTION ( 'NONE',  ( 0.000000000000000000, 1.000000000000000000, 1.795949010423047620E-16 ) ) ;
#6703 = ADVANCED_FACE ( 'NONE', ( #3045, #4566 ), #7058, .T. ) ;
#6704 = CARTESIAN_POINT ( 'NONE',  ( -5.500000000000000000, 6.735557395310442023E-16, -50.00000000000000000 ) ) ;
#6705 = EDGE_CURVE ( 'NONE', #5152, #8094, #4986, .T. ) ;
#6706 = CARTESIAN_POINT ( 'NONE',  ( -8.000000000000227374, 3.115336682266930168, -8.080606868608406046 ) ) ;
#6707 = EDGE_LOOP ( 'NONE', ( #6356, #5302, #8313, #393, #8026, #3068 ) ) ;
#6708 =( NAMED_UNIT ( * ) PLANE_ANGLE_UNIT ( ) SI_UNIT ( $, .RADIAN. ) );
#6709 = ORIENTED_EDGE ( 'NONE', *, *, #856, .F. ) ;
#6710 = FACE_OUTER_BOUND ( 'NONE', #1754, .T. ) ;
#6711 = ORIENTED_EDGE ( 'NONE', *, *, #2331, .F. ) ;
#6712 = AXIS2_PLACEMENT_3D ( 'NONE', #5433, #2927, #2398 ) ;
#6713 = DIRECTION ( 'NONE',  ( 3.851859888774471706E-33, -7.598173571352223877E-18, 1.000000000000000000 ) ) ;
#6714 = CARTESIAN_POINT ( 'NONE',  ( 50.00000000000004263, 500.0000000000000000, -50.00000000000000000 ) ) ;
#6715 = DIRECTION ( 'NONE',  ( 1.000000000000000000, -3.549874073494553124E-30, 0.000000000000000000 ) ) ;
#6716 = CARTESIAN_POINT ( 'NONE',  ( 33.00000000000058265, 3.309499999999951481, 7.105427357601001859E-12 ) ) ;
#6717 = EDGE_LOOP ( 'NONE', ( #6996, #2729, #2577, #5026 ) ) ;
#6718 = EDGE_CURVE ( 'NONE', #5384, #1589, #677, .T. ) ;
#6719 = CONICAL_SURFACE ( 'NONE', #2129, 3.047499999999999876, 1.047197551196592524 ) ;
#6720 = EDGE_LOOP ( 'NONE', ( #3502, #4886 ) ) ;
#6721 = AXIS2_PLACEMENT_3D ( 'NONE', #2320, #4333, #1028 ) ;
#6722 = B_SPLINE_CURVE_WITH_KNOTS ( 'NONE', 3,
 ( #7218, #1245, #6562, #601, #8561, #4611 ),
 .UNSPECIFIED., .F., .F.,
 ( 4, 2, 4 ),
 ( 0.008240550023493499812, 0.01057684187039422026, 0.01291313371729494071 ),
 .UNSPECIFIED. ) ;
#6723 = VECTOR ( 'NONE', #4546, 1000.000000000000000 ) ;
#6724 = DIRECTION ( 'NONE',  ( 0.000000000000000000, 0.000000000000000000, -1.000000000000000000 ) ) ;
#6725 = EDGE_CURVE ( 'NONE', #484, #2264, #5851, .T. ) ;
#6726 = VECTOR ( 'NONE', #5704, 1000.000000000000000 ) ;
#6727 = CARTESIAN_POINT ( 'NONE',  ( -64.99999999999945999, 120.0000000000002842, -5.879478934225335676E-29 ) ) ;
#6728 = ORIENTED_EDGE ( 'NONE', *, *, #672, .T. ) ;
#6729 = LINE ( 'NONE', #3275, #2357 ) ;
#6730 = VECTOR ( 'NONE', #1761, 1000.000000000000000 ) ;
#6731 = DIRECTION ( 'NONE',  ( 0.000000000000000000, 0.000000000000000000, -1.000000000000000000 ) ) ;
#6732 = SHAPE_REPRESENTATION_RELATIONSHIP ( 'NONE' , 'NONE' ,  #2397, #1361 ) ;
#6733 = ORIENTED_EDGE ( 'NONE', *, *, #7134, .T. ) ;
#6734 = FACE_OUTER_BOUND ( 'NONE', #1607, .T. ) ;
#6735 = VERTEX_POINT ( 'NONE', #5221 ) ;
#6736 = AXIS2_PLACEMENT_3D ( 'NONE', #1449, #843, #4105 ) ;
#6737 = DIRECTION ( 'NONE',  ( 0.000000000000000000, 0.000000000000000000, 1.000000000000000000 ) ) ;
#6738 = VECTOR ( 'NONE', #4556, 1000.000000000000000 ) ;
#6739 = EDGE_CURVE ( 'NONE', #3139, #2305, #531, .T. ) ;
#6740 = FACE_OUTER_BOUND ( 'NONE', #7898, .T. ) ;
#6741 = CARTESIAN_POINT ( 'NONE',  ( 10.40000000000001990, 0.000000000000000000, 4.440892098500626162E-13 ) ) ;
#6742 = ORIENTED_EDGE ( 'NONE', *, *, #5598, .T. ) ;
#6743 = CARTESIAN_POINT ( 'NONE',  ( 0.000000000000000000, 410.0000000000000000, -5.551115123125782702E-14 ) ) ;
#6744 = FACE_OUTER_BOUND ( 'NONE', #7939, .T. ) ;
#6745 = CARTESIAN_POINT ( 'NONE',  ( -0.6527133886629282733, 8.860760056385709404, -0.4969600502617304016 ) ) ;
#6746 = AXIS2_PLACEMENT_3D ( 'NONE', #7508, #1534, #4845 ) ;
#6747 = DIRECTION ( 'NONE',  ( 0.000000000000000000, 0.000000000000000000, -1.000000000000000000 ) ) ;
#6748 = VERTEX_POINT ( 'NONE', #3863 ) ;
#6749 = DIRECTION ( 'NONE',  ( 1.463706757734299248E-32, -1.000000000000000000, 4.930380657631321594E-32 ) ) ;
#6750 = PRODUCT_RELATED_PRODUCT_CATEGORY ( 'part', '', ( #1179 ) ) ;
#6751 = EDGE_CURVE ( 'NONE', #2336, #4141, #5009, .T. ) ;
#6752 = CARTESIAN_POINT ( 'NONE',  ( -4.000000000000114575, -6.928203230275542523, 0.000000000000000000 ) ) ;
#6753 = VECTOR ( 'NONE', #5311, 1000.000000000000000 ) ;
#6754 = CARTESIAN_POINT ( 'NONE',  ( 3.999999999999337419, -6.928203230275431501, -8.400000000000018119 ) ) ;
#6755 = CARTESIAN_POINT ( 'NONE',  ( -99.99999999999972999, 0.000000000000000000, 9.999999999999980460 ) ) ;
#6756 = ITEM_DEFINED_TRANSFORMATION ( 'NONE', 'NONE', #2288,  #7563 ) ;
#6757 = CARTESIAN_POINT ( 'NONE',  ( 7.345652830558768720, -4.996589667937484158, -0.4964154566688325776 ) ) ;
#6758 = CARTESIAN_POINT ( 'NONE',  ( -4.000000000000003553, 6.928203230275209457, -8.400000000000018119 ) ) ;
#6759 = ORIENTED_EDGE ( 'NONE', *, *, #7319, .T. ) ;
#6760 = CARTESIAN_POINT ( 'NONE',  ( 0.000000000000000000, -32.50000000000004974, 18.00000000000000355 ) ) ;
#6761 = ORIENTED_EDGE ( 'NONE', *, *, #7578, .T. ) ;
#6762 = DIRECTION ( 'NONE',  ( -1.000000000000000000, -8.881784197001244435E-16, 0.000000000000000000 ) ) ;
#6763 = DIRECTION ( 'NONE',  ( 6.938893903907228378E-17, 0.000000000000000000, -1.000000000000000000 ) ) ;
#6764 = EDGE_CURVE ( 'NONE', #1241, #6892, #3318, .T. ) ;
#6765 = CYLINDRICAL_SURFACE ( 'NONE', #3091, 4.499999999999993783 ) ;
#6766 = CARTESIAN_POINT ( 'NONE',  ( 8.000000000000008882, 3.115336682266734325, -0.3193931313914511461 ) ) ;
#6767 = CARTESIAN_POINT ( 'NONE',  ( -4.250000000000000888, 32.50000000000005684, 18.00000000000000355 ) ) ;
#6768 = LINE ( 'NONE', #6893, #8198 ) ;
#6769 = EDGE_LOOP ( 'NONE', ( #4724, #7181 ) ) ;
#6770 = AXIS2_PLACEMENT_3D ( 'NONE', #3042, #6371, #2432 ) ;
#6771 = ORIENTED_EDGE ( 'NONE', *, *, #4833, .T. ) ;
#6772 = PRODUCT_DEFINITION_SHAPE ( 'NONE', 'NONE',  #8285 ) ;
#6773 = EDGE_CURVE ( 'NONE', #5363, #5659, #5855, .T. ) ;
#6774 = VECTOR ( 'NONE', #4701, 1000.000000000000000 ) ;
#6775 = LINE ( 'NONE', #3458, #1852 ) ;
#6776 = CARTESIAN_POINT ( 'NONE',  ( 4.000000000000003553, 6.928203230275431501, 0.000000000000000000 ) ) ;
#6777 = ORIENTED_EDGE ( 'NONE', *, *, #3176, .T. ) ;
#6778 = DIRECTION ( 'NONE',  ( 0.000000000000000000, 5.322451846059955323E-30, -1.000000000000000000 ) ) ;
#6779 = CARTESIAN_POINT ( 'NONE',  ( 5.000000000000004441, 4.685197434473897360, 0.000000000000000000 ) ) ;
#6780 = CARTESIAN_POINT ( 'NONE',  ( 350.0000000000001137, -1.096345236817342084E-12, 70.00000000000000000 ) ) ;
#6781 = EDGE_LOOP ( 'NONE', ( #5953, #2918, #6884 ) ) ;
#6782 = CARTESIAN_POINT ( 'NONE',  ( -8.000000000000007105, -4.618802153517065356, -0.7145311798163467287 ) ) ;
#6783 = ORIENTED_EDGE ( 'NONE', *, *, #3725, .F. ) ;
#6784 = CARTESIAN_POINT ( 'NONE',  ( -49.99999999999953815, 120.0000000000003268, 9.999999999999980460 ) ) ;
#6785 = ADVANCED_FACE ( 'NONE', ( #1207 ), #518, .T. ) ;
#6786 = FACE_OUTER_BOUND ( 'NONE', #6932, .T. ) ;
#6787 = DIRECTION ( 'NONE',  ( 1.000000000000000000, 0.000000000000000000, 0.000000000000000000 ) ) ;
#6788 = VERTEX_POINT ( 'NONE', #6408 ) ;
#6789 = VECTOR ( 'NONE', #29, 1000.000000000000114 ) ;
#6790 = DIRECTION ( 'NONE',  ( 1.000000000000000000, -1.774937036747276562E-30, -9.447016907875728896E-60 ) ) ;
#6791 = DIRECTION ( 'NONE',  ( -1.000000000000000000, -2.775557561562891745E-15, 0.000000000000000000 ) ) ;
#6792 = DIRECTION ( 'NONE',  ( -7.703719777548943412E-34, 0.000000000000000000, 1.000000000000000000 ) ) ;
#6793 = ORIENTED_EDGE ( 'NONE', *, *, #8068, .F. ) ;
#6794 = EDGE_CURVE ( 'NONE', #1716, #6290, #7705, .T. ) ;
#6795 = CARTESIAN_POINT ( 'NONE',  ( 4.339467034331236484, 6.732211846623466833, -4.488406411676854877E-14 ) ) ;
#6796 = CARTESIAN_POINT ( 'NONE',  ( 4.000000000000058620, 3.518949890710762585, 2.220446049250313081E-13 ) ) ;
#6797 = DIRECTION ( 'NONE',  ( 6.400024471206996205E-36, -1.000000000000000000, -7.598173571352216173E-18 ) ) ;
#6798 = AXIS2_PLACEMENT_3D ( 'NONE', #243, #288, #2947 ) ;
#6799 = CARTESIAN_POINT ( 'NONE',  ( 0.000000000000000000, 0.000000000000000000, 0.000000000000000000 ) ) ;
#6800 = DIRECTION ( 'NONE',  ( 1.000000000000000000, 0.000000000000000000, -6.938893903907228378E-17 ) ) ;
#6801 = ORIENTED_EDGE ( 'NONE', *, *, #7891, .F. ) ;
#6802 = ADVANCED_FACE ( 'NONE', ( #7876 ), #3084, .T. ) ;
#6803 = CARTESIAN_POINT ( 'NONE',  ( 9.999999999999896971, 0.000000000000000000, 79.99999999999995737 ) ) ;
#6804 = ORIENTED_EDGE ( 'NONE', *, *, #80, .T. ) ;
#6805 = CARTESIAN_POINT ( 'NONE',  ( 4.250000000000000888, -32.50000000000004974, 18.00000000000000355 ) ) ;
#6806 = LINE ( 'NONE', #6032, #6789 ) ;
#6807 = EDGE_LOOP ( 'NONE', ( #6098, #5984, #1619 ) ) ;
#6808 = DIRECTION ( 'NONE',  ( -1.463706757734299248E-32, 1.000000000000000000, 5.238529448733281520E-32 ) ) ;
#6809 = ORIENTED_EDGE ( 'NONE', *, *, #7924, .T. ) ;
#6810 = VECTOR ( 'NONE', #6882, 1000.000000000000000 ) ;
#6811 = EDGE_LOOP ( 'NONE', ( #8186, #6446, #2712, #7014 ) ) ;
#6812 = EDGE_CURVE ( 'NONE', #698, #5464, #1819, .T. ) ;
#6813 = AXIS2_PLACEMENT_3D ( 'NONE', #41, #711, #2539 ) ;
#6814 = CARTESIAN_POINT ( 'NONE',  ( 1.310872448938211754, -8.480771745766627845, -0.3173508448888029410 ) ) ;
#6815 = PLANE ( 'NONE',  #6736 ) ;
#6816 = EDGE_LOOP ( 'NONE', ( #5070, #3514, #3175, #3906 ) ) ;
#6817 = APPLICATION_CONTEXT ( 'automotive_design' ) ;
#6818 = DIRECTION ( 'NONE',  ( -3.919652622816902408E-30, -3.944304526105059027E-30, 1.000000000000000000 ) ) ;
#6819 = EDGE_CURVE ( 'NONE', #6524, #5867, #6522, .T. ) ;
#6820 = DIRECTION ( 'NONE',  ( -5.473822126268816683E-48, -0.8660254037844392627, -0.4999999999999988898 ) ) ;
#6821 = DIRECTION ( 'NONE',  ( 8.486676546022956785E-19, -7.552058405137323239E-18, 1.000000000000000000 ) ) ;
#6822 = EDGE_LOOP ( 'NONE', ( #4891, #1451, #3016, #4381, #2150, #2944 ) ) ;
#6823 = ORIENTED_EDGE ( 'NONE', *, *, #6725, .T. ) ;
#6824 = DIRECTION ( 'NONE',  ( 6.938893903907228378E-17, 0.000000000000000000, -1.000000000000000000 ) ) ;
#6825 = FACE_OUTER_BOUND ( 'NONE', #1006, .T. ) ;
#6826 = ORIENTED_EDGE ( 'NONE', *, *, #3454, .F. ) ;
#6827 = CARTESIAN_POINT ( 'NONE',  ( -49.99999999999949551, 152.5000000000003126, -1.942890293094023946E-13 ) ) ;
#6828 = CARTESIAN_POINT ( 'NONE',  ( -2.309976723937542609, 7.903938623646810768, -0.1306530452037677759 ) ) ;
#6829 = EDGE_CURVE ( 'NONE', #6642, #8150, #826, .T. ) ;
#6830 = VERTEX_POINT ( 'NONE', #556 ) ;
#6831 = VECTOR ( 'NONE', #1575, 1000.000000000000000 ) ;
#6832 = EDGE_CURVE ( 'NONE', #4975, #4775, #3044, .T. ) ;
#6833 =( GEOMETRIC_REPRESENTATION_CONTEXT ( 3 ) GLOBAL_UNCERTAINTY_ASSIGNED_CONTEXT ( ( #3434 ) ) GLOBAL_UNIT_ASSIGNED_CONTEXT ( ( #1265, #5548, #7813 ) ) REPRESENTATION_CONTEXT ( 'NONE', 'WORKASPACE' ) );
#6834 = UNCERTAINTY_MEASURE_WITH_UNIT (LENGTH_MEASURE( 1.000000000000000082E-05 ), #4823, 'distance_accuracy_value', 'NONE');
#6835 = CARTESIAN_POINT ( 'NONE',  ( 50.00000000000004263, -425.0000000000000000, -3.469446951953614189E-15 ) ) ;
#6836 = ADVANCED_FACE ( 'NONE', ( #1954, #4090, #4749 ), #8010, .T. ) ;
#6837 = CARTESIAN_POINT ( 'NONE',  ( 3.660532965668319427, -7.124194613927638642, 1.269962144704687948E-13 ) ) ;
#6838 = DIRECTION ( 'NONE',  ( -1.000000000000000000, 2.842664852890546338E-35, -7.703719777548943412E-34 ) ) ;
#6839 = CARTESIAN_POINT ( 'NONE',  ( -5.355005115540773630, -6.145890662065128573, -8.317753204360139208 ) ) ;
#6840 = CARTESIAN_POINT ( 'NONE',  ( 1.000000000000000888, 0.000000000000000000, 0.000000000000000000 ) ) ;
#6841 = ORIENTED_EDGE ( 'NONE', *, *, #6591, .F. ) ;
#6842 = DIRECTION ( 'NONE',  ( 0.000000000000000000, 0.000000000000000000, -1.000000000000000000 ) ) ;
#6843 = EDGE_LOOP ( 'NONE', ( #8245, #4057, #5712, #293, #3669, #1128 ) ) ;
#6844 = DIRECTION ( 'NONE',  ( 7.703719777548943412E-34, -0.000000000000000000, -1.000000000000000000 ) ) ;
#6845 = DIRECTION ( 'NONE',  ( 0.000000000000000000, -0.4999999999999989453, 0.8660254037844392627 ) ) ;
#6846 = EDGE_CURVE ( 'NONE', #5265, #1795, #4638, .T. ) ;
#6847 = ADVANCED_FACE ( 'NONE', ( #4789 ), #3393, .F. ) ;
#6848 = CARTESIAN_POINT ( 'NONE',  ( 275.0000000000000000, -425.0000000000000000, -80.00000000000000000 ) ) ;
#6849 = CARTESIAN_POINT ( 'NONE',  ( -7.999999999999896083, 4.618802153516899267, -8.400000000000018119 ) ) ;
#6850 = VERTEX_POINT ( 'NONE', #6069 ) ;
#6851 = VERTEX_POINT ( 'NONE', #2654 ) ;
#6852 = CARTESIAN_POINT ( 'NONE',  ( 0.000000000000000000, -32.50000000000004974, 18.00000000000000355 ) ) ;
#6853 =( REPRESENTATION_RELATIONSHIP ('NONE','NONE', #1279, #6969 ) REPRESENTATION_RELATIONSHIP_WITH_TRANSFORMATION ( #110 )SHAPE_REPRESENTATION_RELATIONSHIP( ) );
#6854 = EDGE_CURVE ( 'NONE', #1642, #2701, #2081, .T. ) ;
#6855 = AXIS2_PLACEMENT_3D ( 'NONE', #2748, #4832, #4755 ) ;
#6856 = LINE ( 'NONE', #5463, #6280 ) ;
#6857 = ORIENTED_EDGE ( 'NONE', *, *, #3742, .T. ) ;
#6858 = VECTOR ( 'NONE', #1074, 1000.000000000000000 ) ;
#6859 = LINE ( 'NONE', #2883, #5737 ) ;
#6860 = DIRECTION ( 'NONE',  ( -1.000000000000000000, -8.881784197001244435E-16, 0.000000000000000000 ) ) ;
#6861 = CARTESIAN_POINT ( 'NONE',  ( -350.0000000000000568, 59.99999999999992895, -60.69999999999998153 ) ) ;
#6862 = EDGE_LOOP ( 'NONE', ( #675, #2001, #3274, #1901 ) ) ;
#6863 = VECTOR ( 'NONE', #7317, 1000.000000000000114 ) ;
#6864 = CARTESIAN_POINT ( 'NONE',  ( 5.000000000000115463, 2.342598717236854977, -4.057500000000047180 ) ) ;
#6865 = ORIENTED_EDGE ( 'NONE', *, *, #7389, .F. ) ;
#6866 = CIRCLE ( 'NONE', #4633, 50.00000000000008527 ) ;
#6867 = EDGE_CURVE ( 'NONE', #4067, #6439, #2742, .T. ) ;
#6868 = APPLICATION_CONTEXT ( 'automotive_design' ) ;
#6869 = CARTESIAN_POINT ( 'NONE',  ( 0.000000000000000000, 0.000000000000000000, 50.00000000000000000 ) ) ;
#6870 = CARTESIAN_POINT ( 'NONE',  ( -7.345652830558973889, 4.996589667937345602, -0.4964154566688861459 ) ) ;
#6871 = ORIENTED_EDGE ( 'NONE', *, *, #6998, .F. ) ;
#6872 = CONICAL_SURFACE ( 'NONE', #3098, 8.000000000000007105, 1.047197551196597631 ) ;
#6873 = DIRECTION ( 'NONE',  ( -1.000000000000000000, -8.881784197001244435E-16, 0.000000000000000000 ) ) ;
#6874 = DIRECTION ( 'NONE',  ( 0.000000000000000000, 0.000000000000000000, -1.000000000000000000 ) ) ;
#6875 = ORIENTED_EDGE ( 'NONE', *, *, #5493, .F. ) ;
#6876 = VERTEX_POINT ( 'NONE', #2781 ) ;
#6877 = EDGE_CURVE ( 'NONE', #683, #4883, #8058, .T. ) ;
#6878 = CARTESIAN_POINT ( 'NONE',  ( 0.000000000000000000, 0.000000000000000000, -8.400000000000018119 ) ) ;
#6879 = VECTOR ( 'NONE', #3731, 1000.000000000000114 ) ;
#6880 = FACE_OUTER_BOUND ( 'NONE', #4761, .T. ) ;
#6881 =( GEOMETRIC_REPRESENTATION_CONTEXT ( 3 ) GLOBAL_UNCERTAINTY_ASSIGNED_CONTEXT ( ( #3051 ) ) GLOBAL_UNIT_ASSIGNED_CONTEXT ( ( #945, #5618, #4291 ) ) REPRESENTATION_CONTEXT ( 'NONE', 'WORKASPACE' ) );
#6882 = DIRECTION ( 'NONE',  ( 1.000000000000000000, 2.775557561562898056E-15, -3.821045009664285041E-30 ) ) ;
#6883 = CARTESIAN_POINT ( 'NONE',  ( 0.000000000000000000, 0.000000000000000000, 0.000000000000000000 ) ) ;
#6884 = ORIENTED_EDGE ( 'NONE', *, *, #7306, .T. ) ;
#6885 = CARTESIAN_POINT ( 'NONE',  ( -7.999999999999896083, 4.618802153516899267, -0.7145311798163467287 ) ) ;
#6886 = ORIENTED_EDGE ( 'NONE', *, *, #4663, .F. ) ;
#6887 = EDGE_CURVE ( 'NONE', #3489, #3109, #7264, .T. ) ;
#6888 = CARTESIAN_POINT ( 'NONE',  ( -8.000000000000005329, 3.115336682267020763, -0.3193931313915108761 ) ) ;
#6889 = EDGE_CURVE ( 'NONE', #2131, #3105, #1184, .T. ) ;
#6890 = CARTESIAN_POINT ( 'NONE',  ( 4.000000000000003553, 9.714451465470119729E-14, 0.000000000000000000 ) ) ;
#6891 = CARTESIAN_POINT ( 'NONE',  ( 0.000000000000000000, 0.000000000000000000, 0.000000000000000000 ) ) ;
#6892 = VERTEX_POINT ( 'NONE', #8049 ) ;
#6893 = CARTESIAN_POINT ( 'NONE',  ( 44.99999999999992895, 500.0000000000000000, 50.00000000000000000 ) ) ;
#6894 = ORIENTED_EDGE ( 'NONE', *, *, #1872, .F. ) ;
#6895 = ORIENTED_EDGE ( 'NONE', *, *, #2793, .T. ) ;
#6896 = VECTOR ( 'NONE', #7129, 1000.000000000000000 ) ;
#6897 = PLANE ( 'NONE',  #6586 ) ;
#6898 = CARTESIAN_POINT ( 'NONE',  ( 5.000000000000004441, -4.685197434473812095, 0.000000000000000000 ) ) ;
#6899 = ORIENTED_EDGE ( 'NONE', *, *, #4431, .F. ) ;
#6900 = CARTESIAN_POINT ( 'NONE',  ( -50.00000000000004263, 425.0000000000000000, 3.469446951953614189E-15 ) ) ;
#6901 = DIRECTION ( 'NONE',  ( -3.851859888774471706E-33, -1.232595164407830946E-32, -1.000000000000000000 ) ) ;
#6902 = DIRECTION ( 'NONE',  ( -1.000000000000000000, 0.000000000000000000, 0.000000000000000000 ) ) ;
#6903 = EDGE_LOOP ( 'NONE', ( #3252, #42, #6530, #8373 ) ) ;
#6904 = EDGE_CURVE ( 'NONE', #1223, #462, #7947, .T. ) ;
#6905 = DIRECTION ( 'NONE',  ( -1.000000000000000000, -8.881784197001244435E-16, 0.000000000000000000 ) ) ;
#6906 = AXIS2_PLACEMENT_3D ( 'NONE', #289, #4866, #7528 ) ;
#6907 = B_SPLINE_CURVE_WITH_KNOTS ( 'NONE', 3,
 ( #7436, #2130, #5301, #2030, #6606, #2736, #3946, #7255 ),
 .UNSPECIFIED., .F., .F.,
 ( 4, 2, 2, 4 ),
 ( 0.004673709593152171327, 0.005837709341827673759, 0.007001709090503176192, 0.009329708587854181057 ),
 .UNSPECIFIED. ) ;
#6908 = ORIENTED_EDGE ( 'NONE', *, *, #1100, .T. ) ;
#6909 = FACE_OUTER_BOUND ( 'NONE', #1429, .T. ) ;
#6910 = DIRECTION ( 'NONE',  ( -0.9237280213470678847, -0.3830490080632384942, 0.000000000000000000 ) ) ;
#6911 = DIRECTION ( 'NONE',  ( -1.000000000000000000, -6.217248937900875838E-15, 0.000000000000000000 ) ) ;
#6912 = EDGE_LOOP ( 'NONE', ( #5881, #6742 ) ) ;
#6913 = CIRCLE ( 'NONE', #505, 39.75000000000007105 ) ;
#6914 = DIRECTION ( 'NONE',  ( 0.000000000000000000, 5.322451846059955323E-30, -1.000000000000000000 ) ) ;
#6915 = PRESENTATION_LAYER_ASSIGNMENT (  '', '', ( #5820 ) ) ;
#6916 =( NAMED_UNIT ( * ) PLANE_ANGLE_UNIT ( ) SI_UNIT ( $, .RADIAN. ) );
#6917 = EDGE_LOOP ( 'NONE', ( #4011, #8326, #5202, #1252 ) ) ;
#6918 = EDGE_CURVE ( 'NONE', #303, #5323, #1388, .T. ) ;
#6919 = EDGE_LOOP ( 'NONE', ( #3039, #1973, #1020, #191, #3218, #850 ) ) ;
#6920 = VECTOR ( 'NONE', #7902, 1000.000000000000000 ) ;
#6921 = CARTESIAN_POINT ( 'NONE',  ( -17.49999999999958078, 120.0000000000003268, 0.000000000000000000 ) ) ;
#6922 = CARTESIAN_POINT ( 'NONE',  ( -5.690023276062435187, -5.952467836904131282, -0.1306530452038156265 ) ) ;
#6923 = PLANE ( 'NONE',  #7461 ) ;
#6924 = LINE ( 'NONE', #2903, #2529 ) ;
#6925 = FILL_AREA_STYLE ('',( #4826 ) ) ;
#6926 = CARTESIAN_POINT ( 'NONE',  ( 0.000000000000000000, 0.000000000000000000, -8.400000000000018119 ) ) ;
#6927 = ADVANCED_FACE ( 'NONE', ( #648 ), #1380, .T. ) ;
#6928 = FACE_OUTER_BOUND ( 'NONE', #2200, .T. ) ;
#6929 = ORIENTED_EDGE ( 'NONE', *, *, #1759, .T. ) ;
#6930 = EDGE_CURVE ( 'NONE', #3622, #7164, #6669, .T. ) ;
#6931 = CARTESIAN_POINT ( 'NONE',  ( 7.999999999999340972, -4.618802153516732290, -0.7145311798163467287 ) ) ;
#6932 = EDGE_LOOP ( 'NONE', ( #2928, #3133, #1324, #6049 ) ) ;
#6933 = DIRECTION ( 'NONE',  ( 0.000000000000000000, -5.322451846059955323E-30, 1.000000000000000000 ) ) ;
#6934 = CYLINDRICAL_SURFACE ( 'NONE', #4567, 4.250000000000008882 ) ;
#6935 = ORIENTED_EDGE ( 'NONE', *, *, #3774, .F. ) ;
#6936 = VERTEX_POINT ( 'NONE', #3439 ) ;
#6937 = EDGE_CURVE ( 'NONE', #3348, #1467, #2140, .T. ) ;
#6938 = CARTESIAN_POINT ( 'NONE',  ( 5.000000000000004441, 4.685197434473897360, 0.000000000000000000 ) ) ;
#6939 = EDGE_CURVE ( 'NONE', #3109, #1467, #6262, .T. ) ;
#6940 = DIRECTION ( 'NONE',  ( -1.000000000000000000, 0.000000000000000000, 0.000000000000000000 ) ) ;
#6941 = CARTESIAN_POINT ( 'NONE',  ( 8.000000000000117240, 4.618802153517009401, -7.685468820183672278 ) ) ;
#6942 = ORIENTED_EDGE ( 'NONE', *, *, #498, .F. ) ;
#6943 = CARTESIAN_POINT ( 'NONE',  ( 0.6527133886630634985, -8.860760056385847960, -7.903039949738205117 ) ) ;
#6944 = AXIS2_PLACEMENT_3D ( 'NONE', #3825, #7786, #5044 ) ;
#6945 = LINE ( 'NONE', #975, #6137 ) ;
#6946 = DIRECTION ( 'NONE',  ( 0.000000000000000000, 0.000000000000000000, 1.000000000000000000 ) ) ;
#6947 = ORIENTED_EDGE ( 'NONE', *, *, #4908, .F. ) ;
#6948 = AXIS2_PLACEMENT_3D ( 'NONE', #5919, #84, #754 ) ;
#6949 = DIRECTION ( 'NONE',  ( -1.000000000000000000, 0.000000000000000000, -6.938893903907228378E-17 ) ) ;
#6950 = ORIENTED_EDGE ( 'NONE', *, *, #3690, .T. ) ;
#6951 = DIRECTION ( 'NONE',  ( -1.000000000000000000, 3.549874073494553124E-30, 0.000000000000000000 ) ) ;
#6952 = ADVANCED_FACE ( 'NONE', ( #7572 ), #157, .T. ) ;
#6953 = LINE ( 'NONE', #8085, #226 ) ;
#6954 = VERTEX_POINT ( 'NONE', #6972 ) ;
#6955 = DIRECTION ( 'NONE',  ( -1.000000000000000000, -8.881784197001244435E-16, 0.000000000000000000 ) ) ;
#6956 = ORIENTED_EDGE ( 'NONE', *, *, #964, .T. ) ;
#6957 = VECTOR ( 'NONE', #7951, 1000.000000000000000 ) ;
#6958 = AXIS2_PLACEMENT_3D ( 'NONE', #6622, #1138, #5140 ) ;
#6959 = EDGE_LOOP ( 'NONE', ( #8555, #6809, #4075, #5539 ) ) ;
#6960 = CARTESIAN_POINT ( 'NONE',  ( 0.000000000000000000, 0.000000000000000000, 0.000000000000000000 ) ) ;
#6961 = CIRCLE ( 'NONE', #7506, 8.000000000000007105 ) ;
#6962 = B_SPLINE_CURVE_WITH_KNOTS ( 'NONE', 3,
 ( #118, #7535, #1479, #2786, #6158, #5454 ),
 .UNSPECIFIED., .F., .F.,
 ( 4, 2, 4 ),
 ( 2.380731628247750877E-07, 0.002336973833157300531, 0.004673709593151774075 ),
 .UNSPECIFIED. ) ;
#6963 = CIRCLE ( 'NONE', #4862, 8.000000000000007105 ) ;
#6964 = CARTESIAN_POINT ( 'NONE',  ( 8.000000000000008882, 3.871967595401859974, -0.4989386132323923584 ) ) ;
#6965 = CARTESIAN_POINT ( 'NONE',  ( 4.059252933785728601E-13, 119.9999999999998863, 10.00000000000000888 ) ) ;
#6966 = AXIS2_PLACEMENT_3D ( 'NONE', #1839, #1144, #7001 ) ;
#6967 = LINE ( 'NONE', #1510, #2026 ) ;
#6968 = EDGE_CURVE ( 'NONE', #2641, #1999, #4305, .T. ) ;
#6969 = SHAPE_REPRESENTATION ( 'socket head cap screw_am_B18.3.1M - 8 x 1.25 x 25 Hex SHCS -- 25NHX', ( #7563 ), #4234 ) ;
#6970 = PLANE ( 'NONE',  #8103 ) ;
#6971 = VECTOR ( 'NONE', #7699, 1000.000000000000000 ) ;
#6972 = CARTESIAN_POINT ( 'NONE',  ( 10.00000000000012079, -29.14213562373080180, 79.99999999999995737 ) ) ;
#6973 = CARTESIAN_POINT ( 'NONE',  ( 275.0000000000000000, 425.0000000000000000, -74.99999999999984368 ) ) ;
#6974 = DIRECTION ( 'NONE',  ( -1.000000000000000000, -8.881784197001244435E-16, -0.000000000000000000 ) ) ;
#6975 = ORIENTED_EDGE ( 'NONE', *, *, #8357, .T. ) ;
#6976 =( GEOMETRIC_REPRESENTATION_CONTEXT ( 3 ) GLOBAL_UNCERTAINTY_ASSIGNED_CONTEXT ( ( #5259 ) ) GLOBAL_UNIT_ASSIGNED_CONTEXT ( ( #298, #3447, #166 ) ) REPRESENTATION_CONTEXT ( 'NONE', 'WORKASPACE' ) );
#6977 = DIRECTION ( 'NONE',  ( -1.000000000000000000, 0.000000000000000000, 0.000000000000000000 ) ) ;
#6978 = ORIENTED_EDGE ( 'NONE', *, *, #5571, .T. ) ;
#6979 = AXIS2_PLACEMENT_3D ( 'NONE', #3288, #2643, #3990 ) ;
#6980 = CARTESIAN_POINT ( 'NONE',  ( 7.342598717236914041, 0.000000000000000000, 0.000000000000000000 ) ) ;
#6981 = EDGE_CURVE ( 'NONE', #8461, #363, #890, .T. ) ;
#6982 = CARTESIAN_POINT ( 'NONE',  ( 5.000000000000115463, -14.99999999999990230, 79.99999999999995737 ) ) ;
#6983 = ORIENTED_EDGE ( 'NONE', *, *, #8270, .T. ) ;
#6984 = EDGE_LOOP ( 'NONE', ( #5086, #2521 ) ) ;
#6985 = DIRECTION ( 'NONE',  ( 0.000000000000000000, 0.000000000000000000, -1.000000000000000000 ) ) ;
#6986 = ADVANCED_FACE ( 'NONE', ( #8271 ), #3610, .F. ) ;
#6987 = DIRECTION ( 'NONE',  ( -0.5000000000000041078, 0.8660254037844363761, 0.000000000000000000 ) ) ;
#6988 = CARTESIAN_POINT ( 'NONE',  ( 4.000000000000003553, 6.928203230275431501, 0.000000000000000000 ) ) ;
#6989 = ORIENTED_EDGE ( 'NONE', *, *, #3587, .F. ) ;
#6990 = DIRECTION ( 'NONE',  ( 3.851859888774471706E-33, 1.232595164407830946E-32, 1.000000000000000000 ) ) ;
#6991 = CARTESIAN_POINT ( 'NONE',  ( -39.75000000000000000, -1.165861408448480429E-31, 1.925929944387232350E-31 ) ) ;
#6992 = SHAPE_DEFINITION_REPRESENTATION ( #4384, #1942 ) ;
#6993 = VERTEX_POINT ( 'NONE', #2996 ) ;
#6994 = CYLINDRICAL_SURFACE ( 'NONE', #6679, 5.499999999999999112 ) ;
#6995 = AXIS2_PLACEMENT_3D ( 'NONE', #7654, #5533, #950 ) ;
#6996 = ORIENTED_EDGE ( 'NONE', *, *, #3230, .T. ) ;
#6997 = CARTESIAN_POINT ( 'NONE',  ( 0.000000000000000000, 0.000000000000000000, -8.400000000000018119 ) ) ;
#6998 = EDGE_CURVE ( 'NONE', #1251, #5265, #7627, .T. ) ;
#6999 = DIRECTION ( 'NONE',  ( 3.851859888774471706E-33, -7.598173571352223877E-18, 1.000000000000000000 ) ) ;
#7000 = VERTEX_POINT ( 'NONE', #4303 ) ;
#7001 = DIRECTION ( 'NONE',  ( 0.000000000000000000, 0.000000000000000000, 1.000000000000000000 ) ) ;
#7002 = VECTOR ( 'NONE', #1803, 1000.000000000000000 ) ;
#7003 = ORIENTED_EDGE ( 'NONE', *, *, #5482, .F. ) ;
#7004 = ORIENTED_EDGE ( 'NONE', *, *, #7171, .T. ) ;
#7005 = CARTESIAN_POINT ( 'NONE',  ( 6.720025694767360582E-35, -10.50000000000002132, -7.978082249919844238E-17 ) ) ;
#7006 = PRODUCT_DEFINITION_CONTEXT ( 'detailed design', #7856, 'design' ) ;
#7007 = CIRCLE ( 'NONE', #2686, 8.000000000000007105 ) ;
#7008 = CARTESIAN_POINT ( 'NONE',  ( 4.000000000000003553, -2.639212418033041185, -1.523750000000045901 ) ) ;
#7009 = AXIS2_PLACEMENT_3D ( 'NONE', #3652, #5072, #426 ) ;
#7010 = CARTESIAN_POINT ( 'NONE',  ( 275.0000000000000000, 425.0000000000000000, -79.99999999999984368 ) ) ;
#7011 = DIRECTION ( 'NONE',  ( -0.8660254037844365982, 0.5000000000000035527, -0.000000000000000000 ) ) ;
#7012 = CARTESIAN_POINT ( 'NONE',  ( -77.99999999999947420, 120.0000000000003411, 10.00000000000000888 ) ) ;
#7013 = DIRECTION ( 'NONE',  ( 1.000000000000000000, -1.774937036747276562E-30, 0.000000000000000000 ) ) ;
#7014 = ORIENTED_EDGE ( 'NONE', *, *, #4710, .F. ) ;
#7015 = CARTESIAN_POINT ( 'NONE',  ( -4.250000000000000888, -32.50000000000004974, 1.504632769052525000E-32 ) ) ;
#7016 = EDGE_LOOP ( 'NONE', ( #4356, #2893 ) ) ;
#7017 = PRODUCT_DEFINITION ( 'UNKNOWN', '', #7297, #3240 ) ;
#7018 = VECTOR ( 'NONE', #1399, 1000.000000000000000 ) ;
#7019 = DIRECTION ( 'NONE',  ( 0.000000000000000000, 0.000000000000000000, -1.000000000000000000 ) ) ;
#7020 = DIRECTION ( 'NONE',  ( 0.000000000000000000, -5.322451846059955323E-30, 1.000000000000000000 ) ) ;
#7021 = EDGE_LOOP ( 'NONE', ( #4882, #2755 ) ) ;
#7022 = DIRECTION ( 'NONE',  ( 0.000000000000000000, 0.000000000000000000, 1.000000000000000000 ) ) ;
#7023 = AXIS2_PLACEMENT_3D ( 'NONE', #7423, #6174, #2930 ) ;
#7024 = ADVANCED_FACE ( 'NONE', ( #8311 ), #1553, .T. ) ;
#7025 = FACE_BOUND ( 'NONE', #5795, .T. ) ;
#7026 = CARTESIAN_POINT ( 'NONE',  ( 0.000000000000000000, -1.387778780781445676E-14, -120.0000000000000000 ) ) ;
#7027 = VERTEX_POINT ( 'NONE', #1001 ) ;
#7028 = DIRECTION ( 'NONE',  ( 0.5000000000000035527, 0.8660254037844365982, 0.000000000000000000 ) ) ;
#7029 = PRODUCT_DEFINITION_SHAPE ( 'NONE', 'NONE',  #4673 ) ;
#7030 = AXIS2_PLACEMENT_3D ( 'NONE', #1733, #5692, #3134 ) ;
#7031 = CARTESIAN_POINT ( 'NONE',  ( 0.6527133886625579029, -8.860760056385743155, -7.903039949738283276 ) ) ;
#7032 = PRODUCT_CONTEXT ( 'NONE', #8190, 'mechanical' ) ;
#7033 = DIRECTION ( 'NONE',  ( 0.000000000000000000, 0.000000000000000000, 1.000000000000000000 ) ) ;
#7034 = ADVANCED_FACE ( 'NONE', ( #6279 ), #4980, .F. ) ;
#7035 = CARTESIAN_POINT ( 'NONE',  ( 0.000000000000000000, 0.000000000000000000, 0.000000000000000000 ) ) ;
#7036 = DIRECTION ( 'NONE',  ( -0.000000000000000000, -0.000000000000000000, 1.000000000000000000 ) ) ;
#7037 = VERTEX_POINT ( 'NONE', #2334 ) ;
#7038 = CARTESIAN_POINT ( 'NONE',  ( -2.300000000000024247, 0.000000000000000000, 0.000000000000000000 ) ) ;
#7039 = ORIENTED_EDGE ( 'NONE', *, *, #5380, .T. ) ;
#7040 = EDGE_CURVE ( 'NONE', #4829, #704, #7615, .T. ) ;
#7041 = CARTESIAN_POINT ( 'NONE',  ( 6.689127551061957000, 5.375634714784386148, -8.082649155111475636 ) ) ;
#7042 = VERTEX_POINT ( 'NONE', #4991 ) ;
#7043 = LINE ( 'NONE', #1805, #6879 ) ;
#7044 = FACE_OUTER_BOUND ( 'NONE', #5894, .T. ) ;
#7045 = B_SPLINE_CURVE_WITH_KNOTS ( 'NONE', 3,
 ( #5269, #523, #2664, #5908, #8533, #3177, #5862, #5229 ),
 .UNSPECIFIED., .F., .F.,
 ( 4, 2, 2, 4 ),
 ( 0.004673709593151418457, 0.005837709341827142066, 0.007001709090502865676, 0.009329708587854312896 ),
 .UNSPECIFIED. ) ;
#7046 = DIRECTION ( 'NONE',  ( -1.000000000000000000, 0.000000000000000000, -6.938893903907228378E-17 ) ) ;
#7047 = DIRECTION ( 'NONE',  ( 0.000000000000000000, 5.322451846059955323E-30, -1.000000000000000000 ) ) ;
#7048 = EDGE_CURVE ( 'NONE', #1071, #3827, #4151, .T. ) ;
#7049 = CARTESIAN_POINT ( 'NONE',  ( -5.355005115540942384, -6.145890662064630305, -8.317753204360297303 ) ) ;
#7050 = DIRECTION ( 'NONE',  ( 1.000000000000000000, -1.619075244245011343E-15, -3.722437396511636845E-30 ) ) ;
#7051 = ORIENTED_EDGE ( 'NONE', *, *, #2072, .F. ) ;
#7052 = CIRCLE ( 'NONE', #1488, 38.74999999999999289 ) ;
#7053 = DIRECTION ( 'NONE',  ( 1.000000000000000000, -1.284024588418159550E-35, 0.000000000000000000 ) ) ;
#7054 = EDGE_LOOP ( 'NONE', ( #5480, #6120, #992, #159 ) ) ;
#7055 = AXIS2_PLACEMENT_3D ( 'NONE', #5328, #4678, #130 ) ;
#7056 = DIRECTION ( 'NONE',  ( -3.851859888774471706E-33, 7.598173571352223877E-18, -1.000000000000000000 ) ) ;
#7057 = AXIS2_PLACEMENT_3D ( 'NONE', #3506, #281, #4774 ) ;
#7058 = PLANE ( 'NONE',  #4575 ) ;
#7059 = EDGE_LOOP ( 'NONE', ( #1884, #5083, #3660 ) ) ;
#7060 = AXIS2_PLACEMENT_3D ( 'NONE', #3208, #7304, #7957 ) ;
#7061 = ORIENTED_EDGE ( 'NONE', *, *, #1480, .F. ) ;
#7062 = DIRECTION ( 'NONE',  ( -1.000000000000000000, -8.881784197001244435E-16, 0.000000000000000000 ) ) ;
#7063 = CARTESIAN_POINT ( 'NONE',  ( 15.00000000000000000, 1.836970198721029589E-15, 18.00000000000000355 ) ) ;
#7064 = DIRECTION ( 'NONE',  ( 1.000000000000000000, 8.881784197001244435E-16, 0.000000000000000000 ) ) ;
#7065 = EDGE_CURVE ( 'NONE', #6623, #927, #1675, .T. ) ;
#7066 = ORIENTED_EDGE ( 'NONE', *, *, #8354, .F. ) ;
#7067 = AXIS2_PLACEMENT_3D ( 'NONE', #939, #4286, #8212 ) ;
#7068 = DIRECTION ( 'NONE',  ( -1.463706757734299248E-32, 1.000000000000000000, 5.238529448733281520E-32 ) ) ;
#7069 = CARTESIAN_POINT ( 'NONE',  ( 0.000000000000000000, 0.000000000000000000, -8.400000000000018119 ) ) ;
#7070 = CARTESIAN_POINT ( 'NONE',  ( -455.0000000000001705, 62.50000000000009948, 68.00000000000000000 ) ) ;
#7071 = CARTESIAN_POINT ( 'NONE',  ( -6.686525924292697098, 5.377136764700106930, -8.083279549040241818 ) ) ;
#7072 = DIRECTION ( 'NONE',  ( 0.000000000000000000, 0.000000000000000000, 1.000000000000000000 ) ) ;
#7073 = EDGE_CURVE ( 'NONE', #1650, #5363, #910, .T. ) ;
#7074 = ORIENTED_EDGE ( 'NONE', *, *, #7546, .T. ) ;
#7075 = DIRECTION ( 'NONE',  ( 0.000000000000000000, 5.322451846059955323E-30, -1.000000000000000000 ) ) ;
#7076 =( NAMED_UNIT ( * ) SI_UNIT ( $, .STERADIAN. ) SOLID_ANGLE_UNIT ( ) );
#7077 = ORIENTED_EDGE ( 'NONE', *, *, #7114, .F. ) ;
#7078 = LINE ( 'NONE', #1107, #7002 ) ;
#7079 = ORIENTED_EDGE ( 'NONE', *, *, #4404, .T. ) ;
#7080 = CARTESIAN_POINT ( 'NONE',  ( 3.200012235603505426E-34, -50.00000000000008527, -109.9999999999999574 ) ) ;
#7081 = CONICAL_SURFACE ( 'NONE', #3613, 24.49999999999999645, 0.7853981633974503884 ) ;
#7082 = CARTESIAN_POINT ( 'NONE',  ( -50.00000000000004263, -425.0000000000000000, -25.00000000000000355 ) ) ;
#7083 = DIRECTION ( 'NONE',  ( -1.000000000000000000, -8.881784197001244435E-16, 0.000000000000000000 ) ) ;
#7084 = EDGE_CURVE ( 'NONE', #5338, #4033, #8266, .T. ) ;
#7085 = FACE_OUTER_BOUND ( 'NONE', #7397, .T. ) ;
#7086 = CARTESIAN_POINT ( 'NONE',  ( 3.318518101603081139, 7.321656987762871438, -1.409124011052254044E-14 ) ) ;
#7087 = DIRECTION ( 'NONE',  ( 5.329070518200751394E-15, 0.000000000000000000, -1.000000000000000000 ) ) ;
#7088 = APPLICATION_CONTEXT ( 'automotive_design' ) ;
#7089 = DIRECTION ( 'NONE',  ( 0.000000000000000000, -1.795949010423047620E-16, 1.000000000000000000 ) ) ;
#7090 = VERTEX_POINT ( 'NONE', #4911 ) ;
#7091 = SURFACE_STYLE_USAGE ( .BOTH. , #5255 ) ;
#7092 = ORIENTED_EDGE ( 'NONE', *, *, #2663, .F. ) ;
#7093 = AXIS2_PLACEMENT_3D ( 'NONE', #7642, #6425, #6389 ) ;
#7094 = EDGE_CURVE ( 'NONE', #2959, #4132, #3467, .T. ) ;
#7095 = PRODUCT_DEFINITION_SHAPE ( 'NONE', 'NONE',  #3008 ) ;
#7096 = DIRECTION ( 'NONE',  ( 0.000000000000000000, 0.000000000000000000, 1.000000000000000000 ) ) ;
#7097 = ITEM_DEFINED_TRANSFORMATION ( 'NONE', 'NONE', #8132,  #7563 ) ;
#7098 = PRESENTATION_LAYER_ASSIGNMENT (  '', '', ( #3883 ) ) ;
#7099 = DIRECTION ( 'NONE',  ( 6.400024471206996205E-36, -1.000000000000000000, -7.598173571352216173E-18 ) ) ;
#7100 =( GEOMETRIC_REPRESENTATION_CONTEXT ( 3 ) GLOBAL_UNCERTAINTY_ASSIGNED_CONTEXT ( ( #7670 ) ) GLOBAL_UNIT_ASSIGNED_CONTEXT ( ( #1319, #2056, #5508 ) ) REPRESENTATION_CONTEXT ( 'NONE', 'WORKASPACE' ) );
#7101 = EDGE_LOOP ( 'NONE', ( #124, #7646, #954, #6064, #255 ) ) ;
#7102 = EDGE_CURVE ( 'NONE', #7519, #2870, #2962, .T. ) ;
#7103 = ORIENTED_EDGE ( 'NONE', *, *, #5520, .F. ) ;
#7104 = CARTESIAN_POINT ( 'NONE',  ( 1.110223024625156540E-13, -9.237604307034075646, -8.400000000000018119 ) ) ;
#7105 = VECTOR ( 'NONE', #6017, 1000.000000000000000 ) ;
#7106 = AXIS2_PLACEMENT_3D ( 'NONE', #3736, #7046, #6398 ) ;
#7107 = CARTESIAN_POINT ( 'NONE',  ( 0.000000000000000000, 0.000000000000000000, 0.000000000000000000 ) ) ;
#7108 = CARTESIAN_POINT ( 'NONE',  ( -6.661338147750939243E-13, -9.237604307034130713, -8.400000000000018119 ) ) ;
#7109 = DIRECTION ( 'NONE',  ( 0.000000000000000000, -0.000000000000000000, 1.000000000000000000 ) ) ;
#7110 = ORIENTED_EDGE ( 'NONE', *, *, #972, .T. ) ;
#7111 = CARTESIAN_POINT ( 'NONE',  ( 5.000000000000115463, 7.027796151710889561, -4.057500000000047180 ) ) ;
#7112 = CARTESIAN_POINT ( 'NONE',  ( 0.000000000000000000, -299.9999999999999432, 24.49999999999997158 ) ) ;
#7113 = LINE ( 'NONE', #3014, #420 ) ;
#7114 = EDGE_CURVE ( 'NONE', #3413, #7727, #3872, .T. ) ;
#7115 = PRODUCT_RELATED_PRODUCT_CATEGORY ( 'part', '', ( #7853 ) ) ;
#7116 = CARTESIAN_POINT ( 'NONE',  ( -4.000000000000003553, 6.928203230275209457, 0.000000000000000000 ) ) ;
#7117 = ORIENTED_EDGE ( 'NONE', *, *, #5705, .F. ) ;
#7118 = CARTESIAN_POINT ( 'NONE',  ( -45.49999999999946709, 152.5000000000003126, 9.999999999999786837 ) ) ;
#7119 = CARTESIAN_POINT ( 'NONE',  ( 5.499999999999999112, 60.00000000000000000, -50.00000000000000000 ) ) ;
#7120 = VERTEX_POINT ( 'NONE', #8437 ) ;
#7121 = CARTESIAN_POINT ( 'NONE',  ( 2.220446049250313081E-13, 9.237604307034075646, -0.7145311798163467287 ) ) ;
#7122 = ORIENTED_EDGE ( 'NONE', *, *, #4272, .T. ) ;
#7123 = CARTESIAN_POINT ( 'NONE',  ( -5.499999999999999112, 60.00000000000000000, -50.00000000000000000 ) ) ;
#7124 = ADVANCED_FACE ( 'NONE', ( #3852 ), #2628, .T. ) ;
#7125 =( REPRESENTATION_RELATIONSHIP ('NONE','NONE', #1279, #83 ) REPRESENTATION_RELATIONSHIP_WITH_TRANSFORMATION ( #2469 )SHAPE_REPRESENTATION_RELATIONSHIP( ) );
#7126 = DIRECTION ( 'NONE',  ( 0.8660254037844369313, 0.5000000000000028866, 0.000000000000000000 ) ) ;
#7127 = DIRECTION ( 'NONE',  ( -1.463706757734299248E-32, 1.000000000000000000, 5.238529448733281520E-32 ) ) ;
#7128 = CARTESIAN_POINT ( 'NONE',  ( -4.339467034331259576, -6.732211846623360252, -8.400000000000018119 ) ) ;
#7129 = DIRECTION ( 'NONE',  ( -1.000000000000000000, -0.000000000000000000, -0.000000000000000000 ) ) ;
#7130 = CARTESIAN_POINT ( 'NONE',  ( 6.686525924292292977, -5.377136764700166438, -0.3167204509596151518 ) ) ;
#7131 = EDGE_LOOP ( 'NONE', ( #7353, #3821, #5148 ) ) ;
#7132 = VECTOR ( 'NONE', #466, 1000.000000000000227 ) ;
#7133 = VERTEX_POINT ( 'NONE', #6511 ) ;
#7134 = EDGE_CURVE ( 'NONE', #5352, #3217, #7694, .T. ) ;
#7135 = AXIS2_PLACEMENT_3D ( 'NONE', #3814, #791, #2151 ) ;
#7136 = CIRCLE ( 'NONE', #8252, 8.000000000000007105 ) ;
#7137 = AXIS2_PLACEMENT_3D ( 'NONE', #3062, #4284, #7596 ) ;
#7138 = FACE_OUTER_BOUND ( 'NONE', #2860, .T. ) ;
#7139 = ITEM_DEFINED_TRANSFORMATION ( 'NONE', 'NONE', #7842,  #7563 ) ;
#7140 = CARTESIAN_POINT ( 'NONE',  ( -50.00000000000004263, 500.0000000000000000, 50.00000000000000000 ) ) ;
#7141 = ORIENTED_EDGE ( 'NONE', *, *, #485, .T. ) ;
#7142 = AXIS2_PLACEMENT_3D ( 'NONE', #107, #2777, #155 ) ;
#7143 = ORIENTED_EDGE ( 'NONE', *, *, #4362, .T. ) ;
#7144 = CARTESIAN_POINT ( 'NONE',  ( 0.000000000000000000, 0.000000000000000000, 0.000000000000000000 ) ) ;
#7145 = EDGE_CURVE ( 'NONE', #477, #4124, #4298, .T. ) ;
#7146 = ORIENTED_EDGE ( 'NONE', *, *, #2924, .T. ) ;
#7147 = VECTOR ( 'NONE', #8448, 1000.000000000000114 ) ;
#7148 = EDGE_CURVE ( 'NONE', #8288, #450, #2489, .T. ) ;
#7149 = CARTESIAN_POINT ( 'NONE',  ( 0.000000000000000000, 415.0000000000000000, -4.163336342344337027E-14 ) ) ;
#7150 = CARTESIAN_POINT ( 'NONE',  ( 0.000000000000000000, 0.000000000000000000, 0.000000000000000000 ) ) ;
#7151 = DIRECTION ( 'NONE',  ( 1.885870601543981347E-30, -1.000000000000000000, 7.405124331421681105E-16 ) ) ;
#7152 = SURFACE_STYLE_USAGE ( .BOTH. , #4581 ) ;
#7153 = ORIENTED_EDGE ( 'NONE', *, *, #2667, .T. ) ;
#7154 = DIRECTION ( 'NONE',  ( 0.000000000000000000, 5.322451846059955323E-30, -1.000000000000000000 ) ) ;
#7155 = EDGE_CURVE ( 'NONE', #4756, #3262, #2082, .T. ) ;
#7156 = CARTESIAN_POINT ( 'NONE',  ( -2.309976723938476972, 7.903938623647078998, -8.269346954795947724 ) ) ;
#7157 = DIRECTION ( 'NONE',  ( -3.919652622816902408E-30, -3.944304526105059027E-30, 1.000000000000000000 ) ) ;
#7158 = ORIENTED_EDGE ( 'NONE', *, *, #7761, .T. ) ;
#7159 = PLANE ( 'NONE',  #7368 ) ;
#7160 = ADVANCED_FACE ( 'NONE', ( #472 ), #7816, .F. ) ;
#7161 = ORIENTED_EDGE ( 'NONE', *, *, #7171, .F. ) ;
#7162 = CARTESIAN_POINT ( 'NONE',  ( -5.499999999999880096, -14.99999999999990052, -20.00000000000001776 ) ) ;
#7163 = PRODUCT_DEFINITION_SHAPE ( 'NONE', 'NONE',  #7643 ) ;
#7164 = VERTEX_POINT ( 'NONE', #4426 ) ;
#7165 = CARTESIAN_POINT ( 'NONE',  ( 4.339467034331238260, 6.732211846623467721, -8.399999999999973710 ) ) ;
#7166 = CIRCLE ( 'NONE', #7030, 4.250000000000006217 ) ;
#7167 = UNCERTAINTY_MEASURE_WITH_UNIT (LENGTH_MEASURE( 1.000000000000000082E-05 ), #7330, 'distance_accuracy_value', 'NONE');
#7168 = CARTESIAN_POINT ( 'NONE',  ( 0.000000000000000000, 0.000000000000000000, -8.400000000000018119 ) ) ;
#7169 = CARTESIAN_POINT ( 'NONE',  ( 139.1719999999995423, 3.469446951953611664E-14, 4.999999999998625988 ) ) ;
#7170 = CARTESIAN_POINT ( 'NONE',  ( 8.000000000000008882, 3.871967595402187268, -0.4989386132324758472 ) ) ;
#7171 = EDGE_CURVE ( 'NONE', #5811, #3646, #115, .T. ) ;
#7172 = DIRECTION ( 'NONE',  ( 0.000000000000000000, -0.4999999999999983902, 0.8660254037844395958 ) ) ;
#7173 = ORIENTED_EDGE ( 'NONE', *, *, #48, .T. ) ;
#7174 = DIRECTION ( 'NONE',  ( 0.000000000000000000, 0.000000000000000000, -1.000000000000000000 ) ) ;
#7175 = VERTEX_POINT ( 'NONE', #1043 ) ;
#7176 = CARTESIAN_POINT ( 'NONE',  ( 0.000000000000000000, 0.000000000000000000, 0.000000000000000000 ) ) ;
#7177 = CONICAL_SURFACE ( 'NONE', #2581, 8.000000000000007105, 1.047197551196597631 ) ;
#7178 = FILL_AREA_STYLE_COLOUR ( '', #3838 ) ;
#7179 = CARTESIAN_POINT ( 'NONE',  ( 50.00000000000004263, 425.0000000000000000, -3.469446951953614189E-15 ) ) ;
#7180 = ITEM_DEFINED_TRANSFORMATION ( 'NONE', 'NONE', #618,  #7563 ) ;
#7181 = ORIENTED_EDGE ( 'NONE', *, *, #5235, .F. ) ;
#7182 = ADVANCED_FACE ( 'NONE', ( #510 ), #414, .T. ) ;
#7183 = CARTESIAN_POINT ( 'NONE',  ( 0.000000000000000000, 0.000000000000000000, 0.000000000000000000 ) ) ;
#7184 = EDGE_CURVE ( 'NONE', #2953, #5659, #4346, .T. ) ;
#7185 = ORIENTED_EDGE ( 'NONE', *, *, #1461, .F. ) ;
#7186 = LINE ( 'NONE', #3828, #2224 ) ;
#7187 = EDGE_LOOP ( 'NONE', ( #7526, #6477 ) ) ;
#7188 = CARTESIAN_POINT ( 'NONE',  ( 9.999999999999896971, 0.000000000000000000, 0.000000000000000000 ) ) ;
#7189 = VERTEX_POINT ( 'NONE', #3817 ) ;
#7190 = PLANE ( 'NONE',  #3159 ) ;
#7191 = DIRECTION ( 'NONE',  ( -1.000000000000000000, 3.549874073494553124E-30, 0.000000000000000000 ) ) ;
#7192 = DIRECTION ( 'NONE',  ( 0.5000000000000029976, -0.8660254037844370423, 0.000000000000000000 ) ) ;
#7193 = CARTESIAN_POINT ( 'NONE',  ( -7.999999999999896083, -4.618802153517121312, -8.400000000000018119 ) ) ;
#7194 = ORIENTED_EDGE ( 'NONE', *, *, #6043, .F. ) ;
#7195 = EDGE_CURVE ( 'NONE', #6375, #2336, #1698, .T. ) ;
#7196 = APPLICATION_PROTOCOL_DEFINITION ( 'draft international standard', 'automotive_design', 1998, #2157 ) ;
#7197 = DIRECTION ( 'NONE',  ( 1.774937036747276212E-30, -0.5000000000000009992, -0.8660254037844380415 ) ) ;
#7198 = EDGE_CURVE ( 'NONE', #2011, #5903, #8556, .T. ) ;
#7199 = CARTESIAN_POINT ( 'NONE',  ( 0.000000000000000000, 0.000000000000000000, 79.99999999999995737 ) ) ;
#7200 = EDGE_LOOP ( 'NONE', ( #6476, #7592, #5425, #7450 ) ) ;
#7201 = FACE_BOUND ( 'NONE', #4936, .T. ) ;
#7202 = SHAPE_REPRESENTATION_RELATIONSHIP ( 'NONE' , 'NONE' ,  #6969, #6450 ) ;
#7203 = EDGE_LOOP ( 'NONE', ( #7122, #6908, #1590 ) ) ;
#7204 = CARTESIAN_POINT ( 'NONE',  ( -8.000000000000007105, -4.618802153517065356, -8.400000000000018119 ) ) ;
#7205 = EDGE_LOOP ( 'NONE', ( #1476, #3071, #7372, #3595, #596, #4064 ) ) ;
#7206 = CARTESIAN_POINT ( 'NONE',  ( 7.347286611337071172, 4.995646404165302812, -7.903039949738208669 ) ) ;
#7207 = AXIS2_PLACEMENT_3D ( 'NONE', #2960, #2873, #7020 ) ;
#7208 = DIRECTION ( 'NONE',  ( 0.000000000000000000, -0.000000000000000000, 1.000000000000000000 ) ) ;
#7209 = DIRECTION ( 'NONE',  ( 0.000000000000000000, 0.000000000000000000, 1.000000000000000000 ) ) ;
#7210 = DIRECTION ( 'NONE',  ( 8.659560562354897113E-17, 0.7071067811865503483, -0.7071067811865446862 ) ) ;
#7211 = CARTESIAN_POINT ( 'NONE',  ( 8.000000000000229150, -4.440892098500626162E-13, -8.400000000000018119 ) ) ;
#7212 = PLANE ( 'NONE',  #4393 ) ;
#7213 = FACE_OUTER_BOUND ( 'NONE', #1088, .T. ) ;
#7214 = ORIENTED_EDGE ( 'NONE', *, *, #4424, .F. ) ;
#7215 = ORIENTED_EDGE ( 'NONE', *, *, #3145, .T. ) ;
#7216 = CARTESIAN_POINT ( 'NONE',  ( 0.000000000000000000, 0.000000000000000000, 0.000000000000000000 ) ) ;
#7217 = EDGE_CURVE ( 'NONE', #3620, #1712, #6523, .T. ) ;
#7218 = CARTESIAN_POINT ( 'NONE',  ( -8.000000000000007105, -4.618802153517398423, -0.7145311798163467287 ) ) ;
#7219 = CARTESIAN_POINT ( 'NONE',  ( -4.000000000000114575, -6.928203230275487456, -8.400000000000018119 ) ) ;
#7220 = CARTESIAN_POINT ( 'NONE',  ( 0.000000000000000000, 0.000000000000000000, -8.400000000000018119 ) ) ;
#7221 = FACE_BOUND ( 'NONE', #5134, .T. ) ;
#7222 = VERTEX_POINT ( 'NONE', #1157 ) ;
#7223 = DIRECTION ( 'NONE',  ( -7.703719777548943412E-34, 0.000000000000000000, 1.000000000000000000 ) ) ;
#7224 = ORIENTED_EDGE ( 'NONE', *, *, #8268, .T. ) ;
#7225 = ORIENTED_EDGE ( 'NONE', *, *, #5133, .T. ) ;
#7226 = DIRECTION ( 'NONE',  ( -1.000000000000000000, -0.000000000000000000, -0.000000000000000000 ) ) ;
#7227 = ORIENTED_EDGE ( 'NONE', *, *, #7040, .T. ) ;
#7228 = DIRECTION ( 'NONE',  ( -0.9237280213470678847, -0.3830490080632384942, 0.000000000000000000 ) ) ;
#7229 = CIRCLE ( 'NONE', #1387, 4.400000000000030553 ) ;
#7230 = EDGE_CURVE ( 'NONE', #6788, #5411, #1507, .T. ) ;
#7231 = DIRECTION ( 'NONE',  ( 7.420547859534711256E-34, -1.000000000000000000, -1.224646799147352961E-16 ) ) ;
#7232 = AXIS2_PLACEMENT_3D ( 'NONE', #231, #3640, #2279 ) ;
#7233 = CIRCLE ( 'NONE', #1656, 5.559999999999998721 ) ;
#7234 = CARTESIAN_POINT ( 'NONE',  ( 10.00000000000000888, -0.8578643762688908936, 79.99999999999995737 ) ) ;
#7235 = FACE_OUTER_BOUND ( 'NONE', #1606, .T. ) ;
#7236 = ORIENTED_EDGE ( 'NONE', *, *, #732, .T. ) ;
#7237 = DIRECTION ( 'NONE',  ( -0.000000000000000000, -0.000000000000000000, 1.000000000000000000 ) ) ;
#7238 = PRODUCT_DEFINITION_SHAPE ( 'NONE', 'NONE',  #4290 ) ;
#7239 = AXIS2_PLACEMENT_3D ( 'NONE', #6890, #918, #251 ) ;
#7240 = EDGE_CURVE ( 'NONE', #450, #8288, #7640, .T. ) ;
#7241 = CARTESIAN_POINT ( 'NONE',  ( 0.000000000000000000, -3.469446951953614189E-15, 128.9999999999999432 ) ) ;
#7242 = ORIENTED_EDGE ( 'NONE', *, *, #786, .T. ) ;
#7243 = DIRECTION ( 'NONE',  ( -1.000000000000000000, 3.549874073494553124E-30, 0.000000000000000000 ) ) ;
#7244 = DIRECTION ( 'NONE',  ( 0.000000000000000000, 0.000000000000000000, 1.000000000000000000 ) ) ;
#7245 = ORIENTED_EDGE ( 'NONE', *, *, #6386, .F. ) ;
#7246 = FACE_OUTER_BOUND ( 'NONE', #2792, .T. ) ;
#7247 = ORIENTED_EDGE ( 'NONE', *, *, #1007, .F. ) ;
#7248 = CARTESIAN_POINT ( 'NONE',  ( -4.000000000000114575, -6.928203230275487456, 0.000000000000000000 ) ) ;
#7249 = EDGE_CURVE ( 'NONE', #8100, #2145, #2638, .T. ) ;
#7250 = CARTESIAN_POINT ( 'NONE',  ( 0.000000000000000000, 0.000000000000000000, -8.400000000000018119 ) ) ;
#7251 = DIRECTION ( 'NONE',  ( 3.498359009886546906E-15, 1.000000000000000000, -3.747089299799789961E-30 ) ) ;
#7252 = DIRECTION ( 'NONE',  ( 0.000000000000000000, -1.000000000000000000, -7.598173571352217714E-18 ) ) ;
#7253 = DIRECTION ( 'NONE',  ( -0.000000000000000000, -1.000000000000000000, -0.000000000000000000 ) ) ;
#7254 = AXIS2_PLACEMENT_3D ( 'NONE', #6252, #7585, #3425 ) ;
#7255 = CARTESIAN_POINT ( 'NONE',  ( 8.000000000000007105, 4.618802153516899267, -0.7145311798163467287 ) ) ;
#7256 = ORIENTED_EDGE ( 'NONE', *, *, #8184, .F. ) ;
#7257 = CARTESIAN_POINT ( 'NONE',  ( -44.99999999999992895, -425.0000000000000000, 25.00000000000001066 ) ) ;
#7258 = VERTEX_POINT ( 'NONE', #2688 ) ;
#7259 = DIRECTION ( 'NONE',  ( -1.000000000000000000, 3.549874073494553124E-30, 3.778304382545602261E-59 ) ) ;
#7260 = CARTESIAN_POINT ( 'NONE',  ( -2.645508037661968181, -7.710219529346637124, -0.06809871960545786640 ) ) ;
#7261 = DIRECTION ( 'NONE',  ( -3.919652622816902408E-30, -3.944304526105059027E-30, 1.000000000000000000 ) ) ;
#7262 = ORIENTED_EDGE ( 'NONE', *, *, #2767, .F. ) ;
#7263 = CIRCLE ( 'NONE', #2002, 8.000000000000007105 ) ;
#7264 = LINE ( 'NONE', #7964, #3747 ) ;
#7265 = EDGE_LOOP ( 'NONE', ( #2785, #5312 ) ) ;
#7266 = VECTOR ( 'NONE', #7772, 1000.000000000000227 ) ;
#7267 = ADVANCED_FACE ( 'NONE', ( #7385 ), #1389, .T. ) ;
#7268 = ORIENTED_EDGE ( 'NONE', *, *, #2419, .T. ) ;
#7269 = AXIS2_PLACEMENT_3D ( 'NONE', #2832, #8146, #874 ) ;
#7270 = SHAPE_REPRESENTATION ( 'Motor mount pad', ( #7563 ), #2705 ) ;
#7271 = CARTESIAN_POINT ( 'NONE',  ( -8.000000000000117240, -1.110223024625156540E-13, -8.400000000000018119 ) ) ;
#7272 = ORIENTED_EDGE ( 'NONE', *, *, #8572, .T. ) ;
#7273 = CONICAL_SURFACE ( 'NONE', #2538, 8.000000000000007105, 1.047197551196597631 ) ;
#7274 = CARTESIAN_POINT ( 'NONE',  ( 275.0000000000000000, -425.0000000000000000, -75.00000000000000000 ) ) ;
#7275 = CARTESIAN_POINT ( 'NONE',  ( -4.000000000000003553, 6.928203230275209457, 0.000000000000000000 ) ) ;
#7276 = CARTESIAN_POINT ( 'NONE',  ( 8.000000000000120792, 1.572549600175473516, -0.06894455525518324024 ) ) ;
#7277 = VECTOR ( 'NONE', #8111, 1000.000000000000000 ) ;
#7278 = CONICAL_SURFACE ( 'NONE', #1991, 5.700000000000001954, 0.7853981633974472798 ) ;
#7279 = DIRECTION ( 'NONE',  ( 1.000000000000000000, 8.881784197001244435E-16, 0.000000000000000000 ) ) ;
#7280 =( NAMED_UNIT ( * ) PLANE_ANGLE_UNIT ( ) SI_UNIT ( $, .RADIAN. ) );
#7281 = ORIENTED_EDGE ( 'NONE', *, *, #2858, .T. ) ;
#7282 = LINE ( 'NONE', #6164, #5487 ) ;
#7283 = CIRCLE ( 'NONE', #3528, 0.4000000000000001887 ) ;
#7284 = ADVANCED_FACE ( 'NONE', ( #6744 ), #4585, .T. ) ;
#7285 = AXIS2_PLACEMENT_3D ( 'NONE', #5633, #4872, #2180 ) ;
#7286 = CONTEXT_DEPENDENT_SHAPE_REPRESENTATION ( #2634, #7380 ) ;
#7287 = CARTESIAN_POINT ( 'NONE',  ( 50.00000000000004263, -500.0000000000000000, 50.00000000000000000 ) ) ;
#7288 = VECTOR ( 'NONE', #5247, 1000.000000000000000 ) ;
#7289 = ORIENTED_EDGE ( 'NONE', *, *, #7626, .F. ) ;
#7290 = CARTESIAN_POINT ( 'NONE',  ( 3.318518101603052273, 7.321656987762953150, -5.096427837039673649E-14 ) ) ;
#7291 = EDGE_CURVE ( 'NONE', #3413, #5665, #1985, .T. ) ;
#7292 = ORIENTED_EDGE ( 'NONE', *, *, #3154, .T. ) ;
#7293 = CYLINDRICAL_SURFACE ( 'NONE', #6177, 15.00000000000002487 ) ;
#7294 = EDGE_LOOP ( 'NONE', ( #6455, #6402 ) ) ;
#7295 = CARTESIAN_POINT ( 'NONE',  ( 7.999999999999563016, -4.618802153517398423, -7.685468820183672278 ) ) ;
#7296 = CARTESIAN_POINT ( 'NONE',  ( 32.30950000000065359, 4.898587196583831638E-16, -3.999999999993177457 ) ) ;
#7297 = PRODUCT_DEFINITION_FORMATION_WITH_SPECIFIED_SOURCE ( 'ANY', '', #1179, .NOT_KNOWN. ) ;
#7298 = LINE ( 'NONE', #5886, #5 ) ;
#7299 = CARTESIAN_POINT ( 'NONE',  ( -8.000000000000007105, 4.618802153517009401, -0.7145311798163467287 ) ) ;
#7300 = ADVANCED_FACE ( 'NONE', ( #2028 ), #4554, .F. ) ;
#7301 = CARTESIAN_POINT ( 'NONE',  ( -5.499999999999881872, -14.99999999999990052, -20.00100000000004741 ) ) ;
#7302 = ORIENTED_EDGE ( 'NONE', *, *, #2285, .T. ) ;
#7303 = ORIENTED_EDGE ( 'NONE', *, *, #7735, .T. ) ;
#7304 = DIRECTION ( 'NONE',  ( -1.000000000000000000, 1.774937036747276562E-30, 0.000000000000000000 ) ) ;
#7305 = CARTESIAN_POINT ( 'NONE',  ( 6.686525924292487488, -5.377136764700389371, -0.3167204509597881246 ) ) ;
#7306 = EDGE_CURVE ( 'NONE', #5405, #6142, #6961, .T. ) ;
#7307 = FACE_OUTER_BOUND ( 'NONE', #1970, .T. ) ;
#7308 = ITEM_DEFINED_TRANSFORMATION ( 'NONE', 'NONE', #6601,  #7563 ) ;
#7309 = DIRECTION ( 'NONE',  ( 0.000000000000000000, 0.000000000000000000, 1.000000000000000000 ) ) ;
#7310 = CARTESIAN_POINT ( 'NONE',  ( 0.000000000000000000, 0.000000000000000000, 0.000000000000000000 ) ) ;
#7311 = EDGE_LOOP ( 'NONE', ( #1914, #1304, #1024 ) ) ;
#7312 = DIRECTION ( 'NONE',  ( 3.851859888774471706E-33, -7.598173571352223877E-18, 1.000000000000000000 ) ) ;
#7313 = ORIENTED_EDGE ( 'NONE', *, *, #455, .T. ) ;
#7314 = LINE ( 'NONE', #4530, #3918 ) ;
#7315 = ORIENTED_EDGE ( 'NONE', *, *, #8404, .F. ) ;
#7316 = DIRECTION ( 'NONE',  ( 1.000000000000000000, 8.881784197001244435E-16, 0.000000000000000000 ) ) ;
#7317 = DIRECTION ( 'NONE',  ( -0.7071067811864648611, 8.659560562356949384E-17, -0.7071067811866301733 ) ) ;
#7318 = CARTESIAN_POINT ( 'NONE',  ( -5.499999999999999112, 60.00000000000000000, 50.00000000000000000 ) ) ;
#7319 = EDGE_CURVE ( 'NONE', #6028, #7472, #3628, .T. ) ;
#7320 = CIRCLE ( 'NONE', #642, 4.499999999999993783 ) ;
#7321 = CARTESIAN_POINT ( 'NONE',  ( 4.000000000000003553, -6.928203230275542523, 0.000000000000000000 ) ) ;
#7322 = DIRECTION ( 'NONE',  ( 0.000000000000000000, -5.322451846059955323E-30, 1.000000000000000000 ) ) ;
#7323 = ORIENTED_EDGE ( 'NONE', *, *, #133, .F. ) ;
#7324 = CARTESIAN_POINT ( 'NONE',  ( 1.110223024625156540E-13, 9.237604307033992157, -8.400000000000018119 ) ) ;
#7325 = ORIENTED_EDGE ( 'NONE', *, *, #3031, .F. ) ;
#7326 = ADVANCED_FACE ( 'NONE', ( #5436 ), #7915, .F. ) ;
#7327 = CARTESIAN_POINT ( 'NONE',  ( 5.000000000000004441, 4.969004387540602357E-16, -4.057500000000000107 ) ) ;
#7328 = ORIENTED_EDGE ( 'NONE', *, *, #8057, .F. ) ;
#7329 = DIRECTION ( 'NONE',  ( -1.000000000000000000, 0.000000000000000000, 0.000000000000000000 ) ) ;
#7330 =( LENGTH_UNIT ( ) NAMED_UNIT ( * ) SI_UNIT ( .MILLI., .METRE. ) );
#7331 = EDGE_LOOP ( 'NONE', ( #7895, #5107, #4009 ) ) ;
#7332 = CARTESIAN_POINT ( 'NONE',  ( 0.000000000000000000, 0.000000000000000000, 0.000000000000000000 ) ) ;
#7333 = EDGE_LOOP ( 'NONE', ( #2965, #8276, #240, #3429 ) ) ;
#7334 = CARTESIAN_POINT ( 'NONE',  ( 5.499999999999999112, 60.00000000000000000, -50.00000000000000000 ) ) ;
#7335 = EDGE_CURVE ( 'NONE', #1650, #2953, #4439, .T. ) ;
#7336 = CARTESIAN_POINT ( 'NONE',  ( 4.000000000000003553, -6.928203230275542523, -8.400000000000018119 ) ) ;
#7337 = CARTESIAN_POINT ( 'NONE',  ( -8.000000000000225597, 1.572549600175544349, -0.06894455525525224060 ) ) ;
#7338 = CARTESIAN_POINT ( 'NONE',  ( 5.000000000000115463, 7.027796151710889561, -4.057500000000047180 ) ) ;
#7339 = LINE ( 'NONE', #1196, #780 ) ;
#7340 = DIRECTION ( 'NONE',  ( -3.851859888774471706E-33, -1.232595164407830946E-32, -1.000000000000000000 ) ) ;
#7341 = ORIENTED_EDGE ( 'NONE', *, *, #2226, .F. ) ;
#7342 = DIRECTION ( 'NONE',  ( 0.000000000000000000, 0.000000000000000000, -1.000000000000000000 ) ) ;
#7343 = UNCERTAINTY_MEASURE_WITH_UNIT (LENGTH_MEASURE( 1.000000000000000082E-05 ), #774, 'distance_accuracy_value', 'NONE');
#7344 = EDGE_CURVE ( 'NONE', #1987, #7754, #7364, .T. ) ;
#7345 = CARTESIAN_POINT ( 'NONE',  ( -44.99999999999992895, 500.0000000000000000, 45.00000000000000711 ) ) ;
#7346 = CARTESIAN_POINT ( 'NONE',  ( -5.355005115540977911, -6.145890662064671162, -8.317753204360263553 ) ) ;
#7347 = DIRECTION ( 'NONE',  ( -0.000000000000000000, -0.000000000000000000, 1.000000000000000000 ) ) ;
#7348 = CARTESIAN_POINT ( 'NONE',  ( -7.999999999999785061, 4.618802153516954334, -7.685468820183672278 ) ) ;
#7349 = DIRECTION ( 'NONE',  ( 2.842664852890546338E-35, -1.000000000000000000, 0.000000000000000000 ) ) ;
#7350 = LINE ( 'NONE', #4661, #6753 ) ;
#7351 = ORIENTED_EDGE ( 'NONE', *, *, #3410, .T. ) ;
#7352 = SURFACE_STYLE_FILL_AREA ( #7399 ) ;
#7353 = ORIENTED_EDGE ( 'NONE', *, *, #4058, .T. ) ;
#7354 = CARTESIAN_POINT ( 'NONE',  ( -4.000000000000114575, -6.928203230275542523, -8.400000000000018119 ) ) ;
#7355 = ORIENTED_EDGE ( 'NONE', *, *, #335, .F. ) ;
#7356 = DIRECTION ( 'NONE',  ( -1.000000000000000000, 0.000000000000000000, 0.000000000000000000 ) ) ;
#7357 = CARTESIAN_POINT ( 'NONE',  ( 8.000000000000007105, 4.618802153516732290, -0.7145311798163467287 ) ) ;
#7358 = AXIS2_PLACEMENT_3D ( 'NONE', #7720, #3064, #3803 ) ;
#7359 = CARTESIAN_POINT ( 'NONE',  ( -5.500000000000000000, 6.735557395310442023E-16, 50.00000000000000000 ) ) ;
#7360 = ORIENTED_EDGE ( 'NONE', *, *, #3202, .T. ) ;
#7361 = AXIS2_PLACEMENT_3D ( 'NONE', #2243, #1501, #4899 ) ;
#7362 = ORIENTED_EDGE ( 'NONE', *, *, #1626, .F. ) ;
#7363 = B_SPLINE_CURVE_WITH_KNOTS ( 'NONE', 3,
 ( #7468, #4147, #8160, #2195, #7505, #1531, #6216, #4188 ),
 .UNSPECIFIED., .F., .F.,
 ( 4, 2, 2, 4 ),
 ( 0.004673709593152062039, 0.005837709341827626922, 0.007001709090503191804, 0.009329708587854326773 ),
 .UNSPECIFIED. ) ;
#7364 = CIRCLE ( 'NONE', #2088, 15.00000000000002487 ) ;
#7365 = EDGE_CURVE ( 'NONE', #6546, #2856, #6013, .T. ) ;
#7366 = B_SPLINE_CURVE_WITH_KNOTS ( 'NONE', 3,
 ( #3981, #7993, #4024, #5961, #2021, #3322, #6093, #3277 ),
 .UNSPECIFIED., .F., .F.,
 ( 4, 2, 2, 4 ),
 ( 0.004673709593152765469, 0.005837709341828116114, 0.007001709090503465890, 0.009329708587854167179 ),
 .UNSPECIFIED. ) ;
#7367 = CIRCLE ( 'NONE', #3885, 5.500000000000023981 ) ;
#7368 = AXIS2_PLACEMENT_3D ( 'NONE', #6499, #501, #5797 ) ;
#7369 = CARTESIAN_POINT ( 'NONE',  ( 0.000000000000000000, -299.9999999999999432, -2.775557561562891351E-14 ) ) ;
#7370 = CIRCLE ( 'NONE', #3627, 4.250000000000008882 ) ;
#7371 = CARTESIAN_POINT ( 'NONE',  ( 8.000000000000229150, -4.440892098500626162E-13, -8.400000000000018119 ) ) ;
#7372 = ORIENTED_EDGE ( 'NONE', *, *, #2779, .F. ) ;
#7373 = CARTESIAN_POINT ( 'NONE',  ( -6.661338147750939243E-13, 9.237604307034352757, -8.400000000000018119 ) ) ;
#7374 = CARTESIAN_POINT ( 'NONE',  ( 139.9999999999994316, 3.469446951953614189E-14, -1.443289932012703503E-12 ) ) ;
#7375 = ORIENTED_EDGE ( 'NONE', *, *, #2517, .T. ) ;
#7376 = EDGE_CURVE ( 'NONE', #3646, #5811, #4310, .T. ) ;
#7377 = EDGE_CURVE ( 'NONE', #6208, #872, #3283, .T. ) ;
#7378 = VECTOR ( 'NONE', #8093, 1000.000000000000000 ) ;
#7379 = DIRECTION ( 'NONE',  ( -1.000000000000000000, 1.284024588418159817E-35, 0.000000000000000000 ) ) ;
#7380 = PRODUCT_DEFINITION_SHAPE ( 'NONE', 'NONE',  #8610 ) ;
#7381 = ORIENTED_EDGE ( 'NONE', *, *, #2561, .T. ) ;
#7382 = CARTESIAN_POINT ( 'NONE',  ( -8.000000000000229150, -4.618802153516843312, -0.7145311798163467287 ) ) ;
#7383 = DIRECTION ( 'NONE',  ( -0.8660254037844362651, -0.5000000000000039968, 0.000000000000000000 ) ) ;
#7384 = B_SPLINE_CURVE_WITH_KNOTS ( 'NONE', 3,
 ( #4197, #6870, #901, #3555, #5561, #7116 ),
 .UNSPECIFIED., .F., .F.,
 ( 4, 2, 4 ),
 ( 2.380731634175322118E-07, 0.002336973833158143606, 0.004673709593152869553 ),
 .UNSPECIFIED. ) ;
#7385 = FACE_OUTER_BOUND ( 'NONE', #8250, .T. ) ;
#7386 = CARTESIAN_POINT ( 'NONE',  ( -79.99999999999972999, 15.00000000000012434, 1.942890293094023946E-13 ) ) ;
#7387 = CYLINDRICAL_SURFACE ( 'NONE', #3802, 5.499999999999999112 ) ;
#7388 = EDGE_LOOP ( 'NONE', ( #5936, #3989, #3902 ) ) ;
#7389 = EDGE_CURVE ( 'NONE', #1496, #5847, #6648, .T. ) ;
#7390 = VERTEX_POINT ( 'NONE', #7299 ) ;
#7391 = LINE ( 'NONE', #6190, #733 ) ;
#7392 = CARTESIAN_POINT ( 'NONE',  ( 4.681481898396449459, -6.534749472788188740, -8.400000000000190425 ) ) ;
#7393 = DIRECTION ( 'NONE',  ( -1.619075244245011540E-15, -1.000000000000000000, 3.747089299799789961E-30 ) ) ;
#7394 = CONTEXT_DEPENDENT_SHAPE_REPRESENTATION ( #5973, #2171 ) ;
#7395 = CARTESIAN_POINT ( 'NONE',  ( 6.686525924292801903, -5.377136764700267690, -0.3167204509598827156 ) ) ;
#7396 = CARTESIAN_POINT ( 'NONE',  ( -2.644994884460001749, 7.710515798486560435, -8.317753204360025521 ) ) ;
#7397 = EDGE_LOOP ( 'NONE', ( #5262, #3741, #2022 ) ) ;
#7398 = ADVANCED_FACE ( 'NONE', ( #3, #5346 ), #2076, .T. ) ;
#7399 = FILL_AREA_STYLE ('',( #4134 ) ) ;
#7400 = EDGE_LOOP ( 'NONE', ( #2268, #5569, #1060 ) ) ;
#7401 = VECTOR ( 'NONE', #2254, 1000.000000000000000 ) ;
#7402 = FACE_OUTER_BOUND ( 'NONE', #3339, .T. ) ;
#7403 = DIRECTION ( 'NONE',  ( 1.000000000000000000, 0.000000000000000000, 0.000000000000000000 ) ) ;
#7404 = DIRECTION ( 'NONE',  ( -0.9237280213470678847, -0.3830490080632384942, 0.000000000000000000 ) ) ;
#7405 = DIRECTION ( 'NONE',  ( -1.000000000000000000, -8.881784197001244435E-16, 0.000000000000000000 ) ) ;
#7406 = ORIENTED_EDGE ( 'NONE', *, *, #2988, .F. ) ;
#7407 =( REPRESENTATION_RELATIONSHIP ('NONE','NONE', #1279, #3455 ) REPRESENTATION_RELATIONSHIP_WITH_TRANSFORMATION ( #3708 )SHAPE_REPRESENTATION_RELATIONSHIP( ) );
#7408 = FACE_OUTER_BOUND ( 'NONE', #6004, .T. ) ;
#7409 = ORIENTED_EDGE ( 'NONE', *, *, #5738, .T. ) ;
#7410 = AXIS2_PLACEMENT_3D ( 'NONE', #570, #3140, #7931 ) ;
#7411 = DIRECTION ( 'NONE',  ( -3.851859888774471706E-33, -1.232595164407830946E-32, -1.000000000000000000 ) ) ;
#7412 = ORIENTED_EDGE ( 'NONE', *, *, #5620, .F. ) ;
#7413 = EDGE_CURVE ( 'NONE', #757, #6636, #548, .T. ) ;
#7414 = EDGE_CURVE ( 'NONE', #3572, #7660, #2491, .T. ) ;
#7415 = VECTOR ( 'NONE', #8433, 1000.000000000000000 ) ;
#7416 = FACE_OUTER_BOUND ( 'NONE', #7054, .T. ) ;
#7417 = EDGE_CURVE ( 'NONE', #1856, #2336, #8468, .T. ) ;
#7418 = CARTESIAN_POINT ( 'NONE',  ( 8.000000000000015987, -3.098204225878657514, -8.084209322808037612 ) ) ;
#7419 = ORIENTED_EDGE ( 'NONE', *, *, #2285, .F. ) ;
#7420 = DIRECTION ( 'NONE',  ( 1.000000000000000000, 0.000000000000000000, 0.000000000000000000 ) ) ;
#7421 = AXIS2_PLACEMENT_3D ( 'NONE', #4998, #6331, #7664 ) ;
#7422 = CARTESIAN_POINT ( 'NONE',  ( 0.000000000000000000, 32.50000000000005684, 18.00000000000000355 ) ) ;
#7423 = CARTESIAN_POINT ( 'NONE',  ( -4.853265481860481408E-16, 424.9999999999997726, 5.030698080332740574E-14 ) ) ;
#7424 = ORIENTED_EDGE ( 'NONE', *, *, #4315, .F. ) ;
#7425 = DIRECTION ( 'NONE',  ( 1.000000000000000000, 3.083952846180994816E-15, 0.000000000000000000 ) ) ;
#7426 = ORIENTED_EDGE ( 'NONE', *, *, #5280, .T. ) ;
#7427 = AXIS2_PLACEMENT_3D ( 'NONE', #7972, #2005, #7316 ) ;
#7428 = FACE_OUTER_BOUND ( 'NONE', #6843, .T. ) ;
#7429 = EDGE_CURVE ( 'NONE', #2959, #3453, #3558, .T. ) ;
#7430 = CARTESIAN_POINT ( 'NONE',  ( -4.250000000000008882, 32.50000000000005684, 18.00000000000000355 ) ) ;
#7431 = ORIENTED_EDGE ( 'NONE', *, *, #3430, .F. ) ;
#7432 = CARTESIAN_POINT ( 'NONE',  ( -4.000000000000891731, 6.928203230275542523, 0.000000000000000000 ) ) ;
#7433 = DIRECTION ( 'NONE',  ( -1.000000000000000000, 1.774937036747276562E-30, 0.000000000000000000 ) ) ;
#7434 = CARTESIAN_POINT ( 'NONE',  ( 0.000000000000000000, 0.000000000000000000, 0.000000000000000000 ) ) ;
#7435 =( GEOMETRIC_REPRESENTATION_CONTEXT ( 3 ) GLOBAL_UNCERTAINTY_ASSIGNED_CONTEXT ( ( #446 ) ) GLOBAL_UNIT_ASSIGNED_CONTEXT ( ( #3151, #7897, #626 ) ) REPRESENTATION_CONTEXT ( 'NONE', 'WORKASPACE' ) );
#7436 = CARTESIAN_POINT ( 'NONE',  ( 4.000000000000114575, 6.928203230275597591, 0.000000000000000000 ) ) ;
#7437 = ORIENTED_EDGE ( 'NONE', *, *, #7155, .F. ) ;
#7438 = CARTESIAN_POINT ( 'NONE',  ( 50.00000000000004263, 500.0000000000000000, -50.00000000000000000 ) ) ;
#7439 =( NAMED_UNIT ( * ) PLANE_ANGLE_UNIT ( ) SI_UNIT ( $, .RADIAN. ) );
#7440 = CARTESIAN_POINT ( 'NONE',  ( -4.339467034331056183, -6.732211846623884277, -1.918902320027780141E-13 ) ) ;
#7441 = UNCERTAINTY_MEASURE_WITH_UNIT (LENGTH_MEASURE( 1.000000000000000082E-05 ), #5032, 'distance_accuracy_value', 'NONE');
#7442 = PRODUCT_DEFINITION_FORMATION_WITH_SPECIFIED_SOURCE ( 'ANY', '', #1050, .NOT_KNOWN. ) ;
#7443 = CARTESIAN_POINT ( 'NONE',  ( 4.000000000000225597, -6.928203230275542523, 0.000000000000000000 ) ) ;
#7444 = FACE_OUTER_BOUND ( 'NONE', #2362, .T. ) ;
#7445 = VECTOR ( 'NONE', #3440, 1000.000000000000000 ) ;
#7446 = CARTESIAN_POINT ( 'NONE',  ( 5.080504117408889186, 2.106769544347817824, 0.000000000000000000 ) ) ;
#7447 = EDGE_CURVE ( 'NONE', #5555, #1769, #4289, .T. ) ;
#7448 = CARTESIAN_POINT ( 'NONE',  ( 5.080504117408895404, 2.106769544347820489, -8.401000000000047763 ) ) ;
#7449 = CARTESIAN_POINT ( 'NONE',  ( -50.00000000000004263, 425.0000000000000000, 3.469446951953614189E-15 ) ) ;
#7450 = ORIENTED_EDGE ( 'NONE', *, *, #3420, .F. ) ;
#7451 = PRODUCT_DEFINITION_SHAPE ( 'NONE', 'NONE',  #8619 ) ;
#7452 = CARTESIAN_POINT ( 'NONE',  ( -8.000000000000669687, -0.7805016046286902265, -3.591589102947684298E-13 ) ) ;
#7453 = VERTEX_POINT ( 'NONE', #2813 ) ;
#7454 = CARTESIAN_POINT ( 'NONE',  ( 0.000000000000000000, 0.000000000000000000, -50.00000000000000000 ) ) ;
#7455 = CARTESIAN_POINT ( 'NONE',  ( -4.000000000000114575, -6.928203230275487456, 0.000000000000000000 ) ) ;
#7456 = DIRECTION ( 'NONE',  ( 6.400024471207000214E-36, -1.000000000000000000, 0.000000000000000000 ) ) ;
#7457 = EDGE_CURVE ( 'NONE', #922, #4232, #6527, .T. ) ;
#7458 = EDGE_LOOP ( 'NONE', ( #1845, #415 ) ) ;
#7459 = CARTESIAN_POINT ( 'NONE',  ( 275.0000000000000000, 425.0000000000000000, 80.00000000000015632 ) ) ;
#7460 = ORIENTED_EDGE ( 'NONE', *, *, #3869, .F. ) ;
#7461 = AXIS2_PLACEMENT_3D ( 'NONE', #4166, #949, #6276 ) ;
#7462 = ORIENTED_EDGE ( 'NONE', *, *, #6794, .F. ) ;
#7463 = CYLINDRICAL_SURFACE ( 'NONE', #7695, 25.00000000000000711 ) ;
#7464 = EDGE_CURVE ( 'NONE', #5439, #2870, #4121, .T. ) ;
#7465 = DIRECTION ( 'NONE',  ( 1.000000000000000000, 8.881784197001244435E-16, 0.000000000000000000 ) ) ;
#7466 = ORIENTED_EDGE ( 'NONE', *, *, #8539, .F. ) ;
#7467 = EDGE_CURVE ( 'NONE', #2305, #4318, #705, .T. ) ;
#7468 = CARTESIAN_POINT ( 'NONE',  ( -4.000000000000003553, 6.928203230275431501, -8.400000000000018119 ) ) ;
#7469 = CIRCLE ( 'NONE', #6633, 5.499999999999999112 ) ;
#7470 = DIRECTION ( 'NONE',  ( -1.000000000000000000, 0.000000000000000000, 0.000000000000000000 ) ) ;
#7471 = VERTEX_POINT ( 'NONE', #5525 ) ;
#7472 = VERTEX_POINT ( 'NONE', #8171 ) ;
#7473 = DIRECTION ( 'NONE',  ( -1.000000000000000000, -2.775557561562916200E-15, 0.000000000000000000 ) ) ;
#7474 = FACE_OUTER_BOUND ( 'NONE', #2464, .T. ) ;
#7475 = EDGE_LOOP ( 'NONE', ( #5613, #7242 ) ) ;
#7476 = CARTESIAN_POINT ( 'NONE',  ( 8.878689293818315596E-15, 299.9999999999999432, 69.99999999999998579 ) ) ;
#7477 = CARTESIAN_POINT ( 'NONE',  ( 8.000000000000238032, -3.867591403079327250, -7.902324684675273936 ) ) ;
#7478 = DIRECTION ( 'NONE',  ( 0.000000000000000000, 0.000000000000000000, 1.000000000000000000 ) ) ;
#7479 = EDGE_LOOP ( 'NONE', ( #715, #3810 ) ) ;
#7480 = B_SPLINE_CURVE_WITH_KNOTS ( 'NONE', 3,
 ( #406, #3057, #5057, #7715, #1744, #3096, #5788, #3394 ),
 .UNSPECIFIED., .F., .F.,
 ( 4, 2, 2, 4 ),
 ( 0.004673709593152172194, 0.005837709341827674626, 0.007001709090503176192, 0.009329708587854181057 ),
 .UNSPECIFIED. ) ;
#7481 = AXIS2_PLACEMENT_3D ( 'NONE', #6223, #1585, #6911 ) ;
#7482 = DIRECTION ( 'NONE',  ( -1.000000000000000000, 1.284024588418159550E-35, 0.000000000000000000 ) ) ;
#7483 = ORIENTED_EDGE ( 'NONE', *, *, #8339, .T. ) ;
#7484 = EDGE_CURVE ( 'NONE', #6113, #4846, #4942, .T. ) ;
#7485 = DIRECTION ( 'NONE',  ( -7.703719777548943412E-34, 0.000000000000000000, 1.000000000000000000 ) ) ;
#7486 = CARTESIAN_POINT ( 'NONE',  ( 2.644994884458586881, -7.710515798486395234, -0.08224679563963162299 ) ) ;
#7487 = DIRECTION ( 'NONE',  ( 3.919652622816902408E-30, 3.944304526105059027E-30, -1.000000000000000000 ) ) ;
#7488 = CARTESIAN_POINT ( 'NONE',  ( 6.686525924292801903, -5.377136764700267690, -8.083279549040137013 ) ) ;
#7489 = CARTESIAN_POINT ( 'NONE',  ( 8.000000000000012434, -0.7805016046295540910, -3.176542958793075869E-14 ) ) ;
#7490 =( LENGTH_UNIT ( ) NAMED_UNIT ( * ) SI_UNIT ( .MILLI., .METRE. ) );
#7491 = ORIENTED_EDGE ( 'NONE', *, *, #6251, .T. ) ;
#7492 = EDGE_CURVE ( 'NONE', #4232, #4496, #2204, .T. ) ;
#7493 = CARTESIAN_POINT ( 'NONE',  ( 44.99999999999992895, 500.0000000000000000, 50.00000000000000000 ) ) ;
#7494 = DIRECTION ( 'NONE',  ( -1.000000000000000000, 1.284024588418159550E-35, 0.000000000000000000 ) ) ;
#7495 = ORIENTED_EDGE ( 'NONE', *, *, #2058, .T. ) ;
#7496 = CARTESIAN_POINT ( 'NONE',  ( -4.681481898397863439, 6.534749472788354829, -8.399999999999629097 ) ) ;
#7497 = EDGE_LOOP ( 'NONE', ( #7236, #5657, #3625, #3463 ) ) ;
#7498 = B_SPLINE_CURVE_WITH_KNOTS ( 'NONE', 3,
 ( #7336, #5964, #6600, #1234, #1891, #6646, #1329, #7948 ),
 .UNSPECIFIED., .F., .F.,
 ( 4, 2, 2, 4 ),
 ( 0.004673709593152068111, 0.005837709341827601768, 0.007001709090503135426, 0.009329708587854201873 ),
 .UNSPECIFIED. ) ;
#7499 = ORIENTED_EDGE ( 'NONE', *, *, #410, .T. ) ;
#7500 = EDGE_CURVE ( 'NONE', #4183, #896, #4030, .T. ) ;
#7501 = AXIS2_PLACEMENT_3D ( 'NONE', #8395, #1812, #6473 ) ;
#7502 = DIRECTION ( 'NONE',  ( 3.851859888774471706E-33, 1.232595164407830946E-32, 1.000000000000000000 ) ) ;
#7503 = EDGE_LOOP ( 'NONE', ( #1095, #6557, #239, #5986 ) ) ;
#7504 = CONICAL_SURFACE ( 'NONE', #7778, 19.49999999999996803, 0.7853981633974507215 ) ;
#7505 = CARTESIAN_POINT ( 'NONE',  ( -2.309976723937542609, 7.903938623646810768, -8.269346954796251481 ) ) ;
#7506 = AXIS2_PLACEMENT_3D ( 'NONE', #4692, #8552, #6555 ) ;
#7507 = FACE_OUTER_BOUND ( 'NONE', #8592, .T. ) ;
#7508 = CARTESIAN_POINT ( 'NONE',  ( 350.0000000000000000, -7.782199906193609795E-14, -60.70000000000002416 ) ) ;
#7509 = ORIENTED_EDGE ( 'NONE', *, *, #6005, .F. ) ;
#7510 = DIRECTION ( 'NONE',  ( 0.000000000000000000, 0.000000000000000000, 1.000000000000000000 ) ) ;
#7511 = EDGE_CURVE ( 'NONE', #7559, #5338, #274, .T. ) ;
#7512 = CIRCLE ( 'NONE', #979, 4.250000000000008882 ) ;
#7513 = ORIENTED_EDGE ( 'NONE', *, *, #3709, .T. ) ;
#7514 = CARTESIAN_POINT ( 'NONE',  ( 3.200012235603505426E-34, -50.00000000000008527, -109.9999999999999574 ) ) ;
#7515 = CARTESIAN_POINT ( 'NONE',  ( 4.000000000000003553, -6.928203230275542523, 0.000000000000000000 ) ) ;
#7516 = CLOSED_SHELL ( 'NONE', ( #7850, #7709, #439, #2942, #6986, #8159, #3785, #3043, #5532, #3561, #522, #5616, #8447, #5938, #6847, #7160, #4143, #2166, #2017, #4810 ) ) ;
#7517 = VECTOR ( 'NONE', #13, 1000.000000000000114 ) ;
#7518 = CARTESIAN_POINT ( 'NONE',  ( -32.49999999999997158, 3.469446951953614189E-15, 18.00000000000000355 ) ) ;
#7519 = VERTEX_POINT ( 'NONE', #990 ) ;
#7520 = CARTESIAN_POINT ( 'NONE',  ( 0.000000000000000000, 0.000000000000000000, -8.400000000000018119 ) ) ;
#7521 = EDGE_CURVE ( 'NONE', #7819, #3380, #4819, .T. ) ;
#7522 = ORIENTED_EDGE ( 'NONE', *, *, #3184, .T. ) ;
#7523 =( GEOMETRIC_REPRESENTATION_CONTEXT ( 3 ) GLOBAL_UNCERTAINTY_ASSIGNED_CONTEXT ( ( #357 ) ) GLOBAL_UNIT_ASSIGNED_CONTEXT ( ( #6514, #8514, #2558 ) ) REPRESENTATION_CONTEXT ( 'NONE', 'WORKASPACE' ) );
#7524 = ADVANCED_FACE ( 'NONE', ( #1544 ), #8215, .F. ) ;
#7525 = ORIENTED_EDGE ( 'NONE', *, *, #5428, .T. ) ;
#7526 = ORIENTED_EDGE ( 'NONE', *, *, #6773, .T. ) ;
#7527 = LINE ( 'NONE', #1550, #178 ) ;
#7528 = DIRECTION ( 'NONE',  ( -1.000000000000000000, -8.881784197001244435E-16, 0.000000000000000000 ) ) ;
#7529 = DIRECTION ( 'NONE',  ( 3.851859888774471706E-33, -7.598173571352220795E-18, 1.000000000000000000 ) ) ;
#7530 = DIRECTION ( 'NONE',  ( -1.000000000000000000, 7.703719777548936406E-31, 0.000000000000000000 ) ) ;
#7531 = LINE ( 'NONE', #6197, #7565 ) ;
#7532 = VERTEX_POINT ( 'NONE', #8130 ) ;
#7533 = CARTESIAN_POINT ( 'NONE',  ( 8.000000000000015987, -3.867591403078991519, -0.4976753153245472294 ) ) ;
#7534 = VERTEX_POINT ( 'NONE', #942 ) ;
#7535 = CARTESIAN_POINT ( 'NONE',  ( -0.6543471694416775897, -8.859816792613825598, -0.4964154566689172321 ) ) ;
#7536 =( REPRESENTATION_RELATIONSHIP ('NONE','NONE', #1279, #6122 ) REPRESENTATION_RELATIONSHIP_WITH_TRANSFORMATION ( #1126 )SHAPE_REPRESENTATION_RELATIONSHIP( ) );
#7537 = CARTESIAN_POINT ( 'NONE',  ( 0.000000000000000000, 0.000000000000000000, 18.00000000000000355 ) ) ;
#7538 = ORIENTED_EDGE ( 'NONE', *, *, #4056, .F. ) ;
#7539 = CARTESIAN_POINT ( 'NONE',  ( 10.00000000000000888, -4.257961476847964258E-29, 8.000000000000444089 ) ) ;
#7540 = ORIENTED_EDGE ( 'NONE', *, *, #1227, .T. ) ;
#7541 = VERTEX_POINT ( 'NONE', #7476 ) ;
#7542 = COLOUR_RGB ( '',0.7921568627450980005, 0.8196078431372548767, 0.9333333333333333481 ) ;
#7543 = FACE_OUTER_BOUND ( 'NONE', #3079, .T. ) ;
#7544 = CARTESIAN_POINT ( 'NONE',  ( -8.000000000000229150, 4.440892098500626162E-13, 0.000000000000000000 ) ) ;
#7545 = AXIS2_PLACEMENT_3D ( 'NONE', #7693, #8352, #4465 ) ;
#7546 = EDGE_CURVE ( 'NONE', #6592, #7587, #4732, .T. ) ;
#7547 = ORIENTED_EDGE ( 'NONE', *, *, #708, .F. ) ;
#7548 = DIRECTION ( 'NONE',  ( 1.000000000000000000, 8.881784197001244435E-16, 0.000000000000000000 ) ) ;
#7549 = DIRECTION ( 'NONE',  ( 0.000000000000000000, -5.908893405598423146E-30, 1.000000000000000000 ) ) ;
#7550 = DIRECTION ( 'NONE',  ( 0.000000000000000000, 0.000000000000000000, 1.000000000000000000 ) ) ;
#7551 = ORIENTED_EDGE ( 'NONE', *, *, #6877, .T. ) ;
#7552 = DIRECTION ( 'NONE',  ( 0.000000000000000000, 0.000000000000000000, -1.000000000000000000 ) ) ;
#7553 = AXIS2_PLACEMENT_3D ( 'NONE', #5368, #6808, #837 ) ;
#7554 = ORIENTED_EDGE ( 'NONE', *, *, #6889, .F. ) ;
#7555 = CARTESIAN_POINT ( 'NONE',  ( 5.499999999999999112, 60.00000000000000000, 45.00000000000000000 ) ) ;
#7556 = EDGE_CURVE ( 'NONE', #5769, #4067, #8479, .T. ) ;
#7557 = DIRECTION ( 'NONE',  ( 0.000000000000000000, 1.795949010423047620E-16, -1.000000000000000000 ) ) ;
#7558 = ADVANCED_FACE ( 'NONE', ( #2172 ), #460, .T. ) ;
#7559 = VERTEX_POINT ( 'NONE', #7722 ) ;
#7560 = AXIS2_PLACEMENT_3D ( 'NONE', #524, #4483, #7598 ) ;
#7561 = CARTESIAN_POINT ( 'NONE',  ( 4.680456609903819398, 6.535341423375429670, -0.01688885742763771361 ) ) ;
#7562 = VERTEX_POINT ( 'NONE', #5751 ) ;
#7563 = AXIS2_PLACEMENT_3D ( 'NONE', #4203, #7478, #3512 ) ;
#7564 = CARTESIAN_POINT ( 'NONE',  ( 0.000000000000000000, -299.9999999999999432, -2.775557561562891351E-14 ) ) ;
#7565 = VECTOR ( 'NONE', #2867, 1000.000000000000000 ) ;
#7566 = EDGE_LOOP ( 'NONE', ( #3667, #5453, #8143 ) ) ;
#7567 = AXIS2_PLACEMENT_3D ( 'NONE', #4879, #169, #3665 ) ;
#7568 = CARTESIAN_POINT ( 'NONE',  ( 0.000000000000000000, -29.14213562373091548, -20.00000000000001776 ) ) ;
#7569 = CARTESIAN_POINT ( 'NONE',  ( 8.000000000000126121, -3.098204225878304907, -8.084209322808050047 ) ) ;
#7570 = EDGE_CURVE ( 'NONE', #7727, #3413, #980, .T. ) ;
#7571 = LINE ( 'NONE', #4167, #7401 ) ;
#7572 = FACE_OUTER_BOUND ( 'NONE', #5432, .T. ) ;
#7573 = DIRECTION ( 'NONE',  ( -3.919652622816902408E-30, -3.944304526105059027E-30, 1.000000000000000000 ) ) ;
#7574 = ORIENTED_EDGE ( 'NONE', *, *, #7748, .F. ) ;
#7575 = CARTESIAN_POINT ( 'NONE',  ( 32.30950000000065359, 0.000000000000000000, 6.883382752675970551E-12 ) ) ;
#7576 = ORIENTED_EDGE ( 'NONE', *, *, #6854, .F. ) ;
#7577 = AXIS2_PLACEMENT_3D ( 'NONE', #6459, #3678, #3015 ) ;
#7578 = EDGE_CURVE ( 'NONE', #2192, #6339, #3108, .T. ) ;
#7579 = CARTESIAN_POINT ( 'NONE',  ( 275.0000000000000000, -425.0000000000000000, 75.00000000000000000 ) ) ;
#7580 = ORIENTED_EDGE ( 'NONE', *, *, #7927, .T. ) ;
#7581 = CARTESIAN_POINT ( 'NONE',  ( -5.499999999999880096, -14.99999999999990052, 79.99999999999995737 ) ) ;
#7582 = ORIENTED_EDGE ( 'NONE', *, *, #3969, .F. ) ;
#7583 = ORIENTED_EDGE ( 'NONE', *, *, #5327, .T. ) ;
#7584 = B_SPLINE_CURVE_WITH_KNOTS ( 'NONE', 3,
 ( #6931, #7533, #6239, #4349, #914, #1083 ),
 .UNSPECIFIED., .F., .F.,
 ( 4, 2, 4 ),
 ( 0.008240550023493711448, 0.01057684187039402424, 0.01291313371729433702 ),
 .UNSPECIFIED. ) ;
#7585 = DIRECTION ( 'NONE',  ( 0.000000000000000000, 0.000000000000000000, 1.000000000000000000 ) ) ;
#7586 = CARTESIAN_POINT ( 'NONE',  ( 4.339467034331170758, 6.732211846623375351, 1.758122761144706510E-14 ) ) ;
#7587 = VERTEX_POINT ( 'NONE', #5101 ) ;
#7588 = VECTOR ( 'NONE', #1238, 1000.000000000000000 ) ;
#7589 = LINE ( 'NONE', #6089, #4034 ) ;
#7590 = PLANE ( 'NONE',  #5997 ) ;
#7591 = DIRECTION ( 'NONE',  ( 0.7235233670772681647, -0.6902998893909607636, -5.827215960727791636E-18 ) ) ;
#7592 = ORIENTED_EDGE ( 'NONE', *, *, #5789, .F. ) ;
#7593 = CARTESIAN_POINT ( 'NONE',  ( 0.000000000000000000, 299.9999999999999432, -70.00000000000015632 ) ) ;
#7594 = CIRCLE ( 'NONE', #4947, 25.00000000000000711 ) ;
#7595 = ORIENTED_EDGE ( 'NONE', *, *, #2988, .T. ) ;
#7596 = DIRECTION ( 'NONE',  ( 0.000000000000000000, -1.213383262747659708E-29, 1.000000000000000000 ) ) ;
#7597 = EDGE_CURVE ( 'NONE', #7714, #8489, #4337, .T. ) ;
#7598 = DIRECTION ( 'NONE',  ( 0.000000000000000000, 0.000000000000000000, -1.000000000000000000 ) ) ;
#7599 = DIRECTION ( 'NONE',  ( 6.938893903907228378E-17, 0.000000000000000000, -1.000000000000000000 ) ) ;
#7600 = ORIENTED_EDGE ( 'NONE', *, *, #7365, .F. ) ;
#7601 = DIRECTION ( 'NONE',  ( -1.000000000000000000, 1.774937036747276562E-30, 0.000000000000000000 ) ) ;
#7602 = AXIS2_PLACEMENT_3D ( 'NONE', #1862, #6613, #3954 ) ;
#7603 = ORIENTED_EDGE ( 'NONE', *, *, #576, .F. ) ;
#7604 = B_SPLINE_CURVE_WITH_KNOTS ( 'NONE', 3,
 ( #469, #3073, #3032, #8350, #3160, #5719 ),
 .UNSPECIFIED., .F., .F.,
 ( 4, 2, 4 ),
 ( 0.01291313371729497193, 0.01525081363757335370, 0.01758849355785173721 ),
 .UNSPECIFIED. ) ;
#7605 = EDGE_CURVE ( 'NONE', #902, #3235, #532, .T. ) ;
#7606 = VERTEX_POINT ( 'NONE', #2495 ) ;
#7607 = DIRECTION ( 'NONE',  ( 6.400024471206997542E-36, -1.000000000000000000, 0.000000000000000000 ) ) ;
#7608 = ADVANCED_FACE ( 'NONE', ( #8381 ), #1033, .F. ) ;
#7609 = TOROIDAL_SURFACE ( 'NONE', #8028, 5.400000000000034994, 0.4000000000000000222 ) ;
#7610 = DIRECTION ( 'NONE',  ( -1.000000000000000000, 3.549874073494553124E-30, 0.000000000000000000 ) ) ;
#7611 = PLANE ( 'NONE',  #6238 ) ;
#7612 = B_SPLINE_CURVE_WITH_KNOTS ( 'NONE', 3,
 ( #6204, #8520, #8562, #1296, #2601, #5395 ),
 .UNSPECIFIED., .F., .F.,
 ( 4, 2, 4 ),
 ( 0.01291313371729461111, 0.01525081363757316288, 0.01758849355785171292 ),
 .UNSPECIFIED. ) ;
#7613 = CARTESIAN_POINT ( 'NONE',  ( 8.878689293818307707E-15, -299.9999999999999432, -69.99999999999998579 ) ) ;
#7614 = FACE_OUTER_BOUND ( 'NONE', #7200, .T. ) ;
#7615 = LINE ( 'NONE', #6153, #6810 ) ;
#7616 = CARTESIAN_POINT ( 'NONE',  ( 1.110223024625156540E-13, 9.237604307033992157, 0.000000000000000000 ) ) ;
#7617 = EDGE_LOOP ( 'NONE', ( #5595, #6801 ) ) ;
#7618 = CARTESIAN_POINT ( 'NONE',  ( 3.660532965668862548, -7.124194613927656405, -2.499488348229032566E-14 ) ) ;
#7619 = ORIENTED_EDGE ( 'NONE', *, *, #7467, .T. ) ;
#7620 = EDGE_CURVE ( 'NONE', #6830, #2192, #6329, .T. ) ;
#7621 = CARTESIAN_POINT ( 'NONE',  ( 0.000000000000000000, 9.237604307034130713, -0.7145311798163467287 ) ) ;
#7622 = CARTESIAN_POINT ( 'NONE',  ( 10.00000000000000888, 0.000000000000000000, 4.440892098500626162E-13 ) ) ;
#7623 = LINE ( 'NONE', #1054, #398 ) ;
#7624 = EDGE_LOOP ( 'NONE', ( #3152, #6210 ) ) ;
#7625 = ORIENTED_EDGE ( 'NONE', *, *, #1714, .T. ) ;
#7626 = EDGE_CURVE ( 'NONE', #2216, #605, #5708, .T. ) ;
#7627 = CIRCLE ( 'NONE', #106, 8.000000000000007105 ) ;
#7628 = DIRECTION ( 'NONE',  ( -1.000000000000000000, 3.549874073494553124E-30, 3.778304382545602261E-59 ) ) ;
#7629 = CARTESIAN_POINT ( 'NONE',  ( -275.0000000000000000, -425.0000000000000000, 75.00000000000000000 ) ) ;
#7630 = ORIENTED_EDGE ( 'NONE', *, *, #6612, .T. ) ;
#7631 = FACE_OUTER_BOUND ( 'NONE', #1491, .T. ) ;
#7632 = CARTESIAN_POINT ( 'NONE',  ( 4.681481898397195529, -6.534749472788381475, -1.776617725548004789E-13 ) ) ;
#7633 = APPLICATION_PROTOCOL_DEFINITION ( 'draft international standard', 'automotive_design', 1998, #1786 ) ;
#7634 = EDGE_LOOP ( 'NONE', ( #1150, #3021, #7110, #6147 ) ) ;
#7635 = CIRCLE ( 'NONE', #829, 25.00000000000000711 ) ;
#7636 = DIRECTION ( 'NONE',  ( 2.644781493090985226E-59, -7.405124331421681105E-16, -1.000000000000000000 ) ) ;
#7637 = EDGE_LOOP ( 'NONE', ( #6133, #5023 ) ) ;
#7638 = CARTESIAN_POINT ( 'NONE',  ( -34.92499999999998295, 1.224646799147353454E-15, -10.00000000000000178 ) ) ;
#7639 = CARTESIAN_POINT ( 'NONE',  ( 2.220446049250313081E-13, -0.8578643762688908936, -20.00000000000001776 ) ) ;
#7640 = CIRCLE ( 'NONE', #2913, 25.00000000000000711 ) ;
#7641 = ORIENTED_EDGE ( 'NONE', *, *, #4946, .F. ) ;
#7642 = CARTESIAN_POINT ( 'NONE',  ( 139.9999999999996305, 4.171999999999862929, -1.443289932012703503E-12 ) ) ;
#7643 = PRODUCT_DEFINITION ( 'UNKNOWN', '', #7442, #540 ) ;
#7644 =( NAMED_UNIT ( * ) SI_UNIT ( $, .STERADIAN. ) SOLID_ANGLE_UNIT ( ) );
#7645 = ORIENTED_EDGE ( 'NONE', *, *, #5204, .F. ) ;
#7646 = ORIENTED_EDGE ( 'NONE', *, *, #1425, .F. ) ;
#7647 = EDGE_LOOP ( 'NONE', ( #5162, #465, #920 ) ) ;
#7648 = CARTESIAN_POINT ( 'NONE',  ( 0.6543471694413474093, 8.859816792613639080, -7.903584543331222179 ) ) ;
#7649 = COLOUR_RGB ( '',0.7921568627450980005, 0.8196078431372548767, 0.9333333333333333481 ) ;
#7650 = CIRCLE ( 'NONE', #5130, 25.00000000000000711 ) ;
#7651 = CARTESIAN_POINT ( 'NONE',  ( -8.000000000000117240, -1.110223024625156540E-13, 0.000000000000000000 ) ) ;
#7652 = DIRECTION ( 'NONE',  ( 1.000000000000000000, -1.284024588418159550E-35, 3.851859888774464864E-33 ) ) ;
#7653 = DIRECTION ( 'NONE',  ( 7.703719777548943412E-34, -0.000000000000000000, -1.000000000000000000 ) ) ;
#7654 = CARTESIAN_POINT ( 'NONE',  ( 0.000000000000000000, 60.00000000000000000, 45.00000000000000000 ) ) ;
#7655 = CONICAL_SURFACE ( 'NONE', #5282, 8.000000000000007105, 1.047197551196597631 ) ;
#7656 = DIRECTION ( 'NONE',  ( 0.000000000000000000, 0.000000000000000000, 1.000000000000000000 ) ) ;
#7657 = ADVANCED_FACE ( 'NONE', ( #7685 ), #7804, .T. ) ;
#7658 = CARTESIAN_POINT ( 'NONE',  ( 4.000000000000003553, -1.759474945355333109, 3.047500000000091802 ) ) ;
#7659 = CARTESIAN_POINT ( 'NONE',  ( 8.000000000000229150, -4.440892098500626162E-13, 0.000000000000000000 ) ) ;
#7660 = VERTEX_POINT ( 'NONE', #6463 ) ;
#7661 = CONICAL_SURFACE ( 'NONE', #8235, 8.000000000000007105, 1.047197551196597631 ) ;
#7662 = FACE_OUTER_BOUND ( 'NONE', #2454, .T. ) ;
#7663 = ORIENTED_EDGE ( 'NONE', *, *, #394, .T. ) ;
#7664 = DIRECTION ( 'NONE',  ( 0.000000000000000000, 1.000000000000000000, 0.000000000000000000 ) ) ;
#7665 = CARTESIAN_POINT ( 'NONE',  ( 0.000000000000000000, 0.000000000000000000, 0.000000000000000000 ) ) ;
#7666 = ORIENTED_EDGE ( 'NONE', *, *, #7735, .F. ) ;
#7667 = ADVANCED_FACE ( 'NONE', ( #8337 ), #7159, .T. ) ;
#7668 = ORIENTED_EDGE ( 'NONE', *, *, #6085, .T. ) ;
#7669 = DIRECTION ( 'NONE',  ( 1.000000000000000000, 2.775557561562892140E-15, -3.821045009664285742E-30 ) ) ;
#7670 = UNCERTAINTY_MEASURE_WITH_UNIT (LENGTH_MEASURE( 1.000000000000000082E-05 ), #1319, 'distance_accuracy_value', 'NONE');
#7671 = VECTOR ( 'NONE', #4825, 1000.000000000000000 ) ;
#7672 = CARTESIAN_POINT ( 'NONE',  ( 1.110223024625156540E-13, 2.342598717236896722, -4.057500000000047180 ) ) ;
#7673 = CARTESIAN_POINT ( 'NONE',  ( 275.0000000000000000, -425.0000000000000000, 75.00000000000000000 ) ) ;
#7674 = ORIENTED_EDGE ( 'NONE', *, *, #8558, .F. ) ;
#7675 = ADVANCED_FACE ( 'NONE', ( #4979 ), #2364, .T. ) ;
#7676 = CARTESIAN_POINT ( 'NONE',  ( 32.49999999999997158, 1.387778780781445676E-14, 18.00000000000000355 ) ) ;
#7677 = CARTESIAN_POINT ( 'NONE',  ( 3.660532965668318983, -7.124194613927635089, -8.400000000000146017 ) ) ;
#7678 = SHAPE_DEFINITION_REPRESENTATION ( #7029, #3167 ) ;
#7679 = DIRECTION ( 'NONE',  ( -0.9237280213470678847, -0.3830490080632384942, 0.000000000000000000 ) ) ;
#7680 = VECTOR ( 'NONE', #5369, 1000.000000000000000 ) ;
#7681 = CARTESIAN_POINT ( 'NONE',  ( -12.99999999999955058, 120.0000000000003411, 9.999999999999980460 ) ) ;
#7682 = VECTOR ( 'NONE', #7226, 1000.000000000000000 ) ;
#7683 = CARTESIAN_POINT ( 'NONE',  ( 4.000000000000003553, 1.759474945355374409, 3.047499999999869758 ) ) ;
#7684 = VERTEX_POINT ( 'NONE', #1664 ) ;
#7685 = FACE_OUTER_BOUND ( 'NONE', #2546, .T. ) ;
#7686 = ORIENTED_EDGE ( 'NONE', *, *, #7148, .F. ) ;
#7687 = CARTESIAN_POINT ( 'NONE',  ( 4.339467034330983353, 6.732211846623264329, -8.400000000000151346 ) ) ;
#7688 = ORIENTED_EDGE ( 'NONE', *, *, #647, .T. ) ;
#7689 = AXIS2_PLACEMENT_3D ( 'NONE', #1740, #3267, #615 ) ;
#7690 = FACE_OUTER_BOUND ( 'NONE', #1226, .T. ) ;
#7691 = CARTESIAN_POINT ( 'NONE',  ( -8.000000000000673239, 4.618802153517287401, -8.400000000000018119 ) ) ;
#7692 = SURFACE_SIDE_STYLE ('',( #2375 ) ) ;
#7693 = CARTESIAN_POINT ( 'NONE',  ( 9.999999999999896971, 0.000000000000000000, 0.000000000000000000 ) ) ;
#7694 = LINE ( 'NONE', #5210, #5123 ) ;
#7695 = AXIS2_PLACEMENT_3D ( 'NONE', #3588, #4885, #6249 ) ;
#7696 = APPLICATION_CONTEXT ( 'automotive_design' ) ;
#7697 = LINE ( 'NONE', #1081, #2154 ) ;
#7698 = ORIENTED_EDGE ( 'NONE', *, *, #8462, .T. ) ;
#7699 = DIRECTION ( 'NONE',  ( -1.000000000000000000, 0.000000000000000000, 0.000000000000000000 ) ) ;
#7700 = ORIENTED_EDGE ( 'NONE', *, *, #6152, .T. ) ;
#7701 = AXIS2_PLACEMENT_3D ( 'NONE', #3564, #241, #775 ) ;
#7702 = EDGE_CURVE ( 'NONE', #3933, #6230, #7233, .T. ) ;
#7703 = CIRCLE ( 'NONE', #8263, 39.75000000000007105 ) ;
#7704 = DIRECTION ( 'NONE',  ( 1.000000000000000000, 0.000000000000000000, -6.938893903907228378E-17 ) ) ;
#7705 = LINE ( 'NONE', #441, #6129 ) ;
#7706 = ORIENTED_EDGE ( 'NONE', *, *, #6415, .T. ) ;
#7707 = FACE_OUTER_BOUND ( 'NONE', #7566, .T. ) ;
#7708 = AXIS2_PLACEMENT_3D ( 'NONE', #5604, #803, #5656 ) ;
#7709 = ADVANCED_FACE ( 'NONE', ( #5022 ), #4457, .F. ) ;
#7710 = EDGE_CURVE ( 'NONE', #4975, #757, #3066, .T. ) ;
#7711 = VECTOR ( 'NONE', #5932, 1000.000000000000000 ) ;
#7712 = DIRECTION ( 'NONE',  ( -1.000000000000000000, 1.774937036747276562E-30, 0.000000000000000000 ) ) ;
#7713 = DIRECTION ( 'NONE',  ( -0.7071067811864648611, -5.015942853701814625E-30, 0.7071067811866301733 ) ) ;
#7714 = VERTEX_POINT ( 'NONE', #3769 ) ;
#7715 = CARTESIAN_POINT ( 'NONE',  ( 5.355005115540955707, 6.145890662064649845, -8.317753204360281316 ) ) ;
#7716 = AXIS2_PLACEMENT_3D ( 'NONE', #5175, #4359, #1869 ) ;
#7717 = CARTESIAN_POINT ( 'NONE',  ( 5.354491962338240540, -6.146186931204690396, -0.06809871960559767123 ) ) ;
#7718 = DIRECTION ( 'NONE',  ( 0.000000000000000000, -1.024214141749972931E-29, 1.000000000000000000 ) ) ;
#7719 = EDGE_CURVE ( 'NONE', #5471, #2816, #5833, .T. ) ;
#7720 = CARTESIAN_POINT ( 'NONE',  ( 0.000000000000000000, 0.000000000000000000, 18.00000000000000355 ) ) ;
#7721 = EDGE_LOOP ( 'NONE', ( #7161, #295 ) ) ;
#7722 = CARTESIAN_POINT ( 'NONE',  ( -8.000000000000007105, 0.000000000000000000, -8.400000000000018119 ) ) ;
#7723 = ORIENTED_EDGE ( 'NONE', *, *, #165, .F. ) ;
#7724 = ADVANCED_FACE ( 'NONE', ( #7201, #3319 ), #8541, .T. ) ;
#7725 = EDGE_CURVE ( 'NONE', #7534, #530, #6729, .T. ) ;
#7726 = CARTESIAN_POINT ( 'NONE',  ( 2.645508037661678191, 7.710219529346706402, -0.06809871960543743830 ) ) ;
#7727 = VERTEX_POINT ( 'NONE', #1366 ) ;
#7728 = CARTESIAN_POINT ( 'NONE',  ( -4.000000000000114575, -6.928203230275487456, -8.400000000000018119 ) ) ;
#7729 = CARTESIAN_POINT ( 'NONE',  ( 9.999999999999896971, 0.000000000000000000, 0.000000000000000000 ) ) ;
#7730 = CARTESIAN_POINT ( 'NONE',  ( -275.0000000000000000, -425.0000000000000000, 0.000000000000000000 ) ) ;
#7731 = CARTESIAN_POINT ( 'NONE',  ( 1.313474075707311339, 8.479269695850856436, -0.3167204509598462447 ) ) ;
#7732 = DIRECTION ( 'NONE',  ( -1.000000000000000000, 0.000000000000000000, 0.000000000000000000 ) ) ;
#7733 = CARTESIAN_POINT ( 'NONE',  ( -0.6527133886628256887, 8.860760056385791117, -7.903039949738245085 ) ) ;
#7734 = EDGE_LOOP ( 'NONE', ( #4150, #4470 ) ) ;
#7735 = EDGE_CURVE ( 'NONE', #1219, #7453, #273, .T. ) ;
#7736 = ADVANCED_FACE ( 'NONE', ( #5957 ), #3928, .T. ) ;
#7737 = AXIS2_PLACEMENT_3D ( 'NONE', #6741, #2636, #8506 ) ;
#7738 = CARTESIAN_POINT ( 'NONE',  ( 5.080504117408889186, 2.106769544347817824, -8.400000000000018119 ) ) ;
#7739 = EDGE_LOOP ( 'NONE', ( #5572, #2242 ) ) ;
#7740 = PRESENTATION_LAYER_ASSIGNMENT (  '', '', ( #4405 ) ) ;
#7741 = CARTESIAN_POINT ( 'NONE',  ( 3.319543390096325375, -7.321065037175607415, -0.01688885742793171801 ) ) ;
#7742 = DIRECTION ( 'NONE',  ( 0.000000000000000000, 1.795949010423047374E-16, -1.000000000000000000 ) ) ;
#7743 = ITEM_DEFINED_TRANSFORMATION ( 'NONE', 'NONE', #5647,  #7563 ) ;
#7744 = DIRECTION ( 'NONE',  ( -1.000000000000000000, 3.549874073494553124E-30, 3.778304382545602261E-59 ) ) ;
#7745 = ORIENTED_EDGE ( 'NONE', *, *, #4961, .F. ) ;
#7746 = ORIENTED_EDGE ( 'NONE', *, *, #4375, .T. ) ;
#7747 = DIRECTION ( 'NONE',  ( -3.919652622816902408E-30, -3.944304526105059027E-30, 1.000000000000000000 ) ) ;
#7748 = EDGE_CURVE ( 'NONE', #3548, #4837, #6046, .T. ) ;
#7749 = PRODUCT_RELATED_PRODUCT_CATEGORY ( 'part', '', ( #8343 ) ) ;
#7750 = UNCERTAINTY_MEASURE_WITH_UNIT (LENGTH_MEASURE( 1.000000000000000082E-05 ), #7929, 'distance_accuracy_value', 'NONE');
#7751 = CARTESIAN_POINT ( 'NONE',  ( 1.110223024625156540E-13, 9.237604307033992157, -8.400000000000018119 ) ) ;
#7752 = CARTESIAN_POINT ( 'NONE',  ( 4.000000000000003553, 1.759474945355374409, 3.047499999999869758 ) ) ;
#7753 = DIRECTION ( 'NONE',  ( -1.540743955509788682E-33, -4.592425496802573602E-17, 1.000000000000000000 ) ) ;
#7754 = VERTEX_POINT ( 'NONE', #43 ) ;
#7755 = DIRECTION ( 'NONE',  ( -0.7071067811864683028, 8.659560562356407042E-17, -0.7071067811866268427 ) ) ;
#7756 = CARTESIAN_POINT ( 'NONE',  ( 2.309976723937648746, -7.903938623646967088, -8.269346954796146676 ) ) ;
#7757 = EDGE_CURVE ( 'NONE', #927, #5835, #6003, .T. ) ;
#7758 = CARTESIAN_POINT ( 'NONE',  ( 4.000000000000225597, -6.928203230275542523, 0.000000000000000000 ) ) ;
#7759 = ORIENTED_EDGE ( 'NONE', *, *, #6887, .T. ) ;
#7760 = CARTESIAN_POINT ( 'NONE',  ( 0.000000000000000000, 0.000000000000000000, 0.000000000000000000 ) ) ;
#7761 = EDGE_CURVE ( 'NONE', #7222, #7833, #5879, .T. ) ;
#7762 = LINE ( 'NONE', #7119, #1944 ) ;
#7763 = ORIENTED_EDGE ( 'NONE', *, *, #1131, .F. ) ;
#7764 = CARTESIAN_POINT ( 'NONE',  ( 0.000000000000000000, 0.000000000000000000, -8.400000000000018119 ) ) ;
#7765 = ORIENTED_EDGE ( 'NONE', *, *, #4754, .T. ) ;
#7766 = CARTESIAN_POINT ( 'NONE',  ( -5.080504117408896292, -2.106769544347821377, 5.551115123125782702E-14 ) ) ;
#7767 = AXIS2_PLACEMENT_3D ( 'NONE', #3298, #1303, #781 ) ;
#7768 = PLANE ( 'NONE',  #4639 ) ;
#7769 = LINE ( 'NONE', #1154, #5523 ) ;
#7770 = DIRECTION ( 'NONE',  ( -1.000000000000000000, 0.000000000000000000, 0.000000000000000000 ) ) ;
#7771 = CONICAL_SURFACE ( 'NONE', #981, 40.00000000000007816, 0.7853981633974445042 ) ;
#7772 = DIRECTION ( 'NONE',  ( 8.659560562354906974E-17, -0.7071067811865454633, -0.7071067811865495711 ) ) ;
#7773 = CARTESIAN_POINT ( 'NONE',  ( 8.000000000000007105, 0.000000000000000000, 0.000000000000000000 ) ) ;
#7774 = CARTESIAN_POINT ( 'NONE',  ( -50.00000000000004263, -425.0000000000000000, 25.00000000000001066 ) ) ;
#7775 = EDGE_CURVE ( 'NONE', #3744, #2338, #2765, .T. ) ;
#7776 = DIRECTION ( 'NONE',  ( 0.000000000000000000, 1.078520768856843950E-29, -1.000000000000000000 ) ) ;
#7777 = EDGE_LOOP ( 'NONE', ( #7582, #8230, #7700, #706, #3917 ) ) ;
#7778 = AXIS2_PLACEMENT_3D ( 'NONE', #2018, #7941, #6731 ) ;
#7779 = EDGE_LOOP ( 'NONE', ( #4616, #2876, #8570, #7146 ) ) ;
#7780 = B_SPLINE_CURVE_WITH_KNOTS ( 'NONE', 3,
 ( #5713, #7687, #1715, #4383, #6392, #7041, #4795, #3729 ),
 .UNSPECIFIED., .F., .F.,
 ( 4, 2, 2, 4 ),
 ( 0.004673709593151988313, 0.005837709341827519369, 0.007001709090503049557, 0.009329708587854111668 ),
 .UNSPECIFIED. ) ;
#7781 = CIRCLE ( 'NONE', #8347, 5.400000000000034994 ) ;
#7782 = AXIS2_PLACEMENT_3D ( 'NONE', #7373, #4543, #4065 ) ;
#7783 = VECTOR ( 'NONE', #1393, 1000.000000000000000 ) ;
#7784 = FACE_OUTER_BOUND ( 'NONE', #7503, .T. ) ;
#7785 = CONTEXT_DEPENDENT_SHAPE_REPRESENTATION ( #7536, #6083 ) ;
#7786 = DIRECTION ( 'NONE',  ( -3.919652622816902408E-30, -3.944304526105059027E-30, 1.000000000000000000 ) ) ;
#7787 = MECHANICAL_DESIGN_GEOMETRIC_PRESENTATION_REPRESENTATION (  '', ( #2791 ), #6976 ) ;
#7788 = ORIENTED_EDGE ( 'NONE', *, *, #769, .F. ) ;
#7789 = AXIS2_PLACEMENT_3D ( 'NONE', #2627, #3187, #7896 ) ;
#7790 = EDGE_LOOP ( 'NONE', ( #7224, #2381, #5945 ) ) ;
#7791 = FACE_BOUND ( 'NONE', #4051, .T. ) ;
#7792 = ORIENTED_EDGE ( 'NONE', *, *, #1216, .T. ) ;
#7793 = CONICAL_SURFACE ( 'NONE', #1049, 8.000000000000007105, 1.047197551196597631 ) ;
#7794 = CYLINDRICAL_SURFACE ( 'NONE', #8314, 4.499999999999990230 ) ;
#7795 = CARTESIAN_POINT ( 'NONE',  ( 1.110223024625156540E-13, 2.342598717236896722, -4.057500000000047180 ) ) ;
#7796 = FILL_AREA_STYLE_COLOUR ( '', #7542 ) ;
#7797 = EDGE_LOOP ( 'NONE', ( #2907, #4245, #4994, #7574 ) ) ;
#7798 = CARTESIAN_POINT ( 'NONE',  ( 0.000000000000000000, 415.0000000000000000, -19.50000000000002487 ) ) ;
#7799 = LINE ( 'NONE', #365, #2780 ) ;
#7800 = DIRECTION ( 'NONE',  ( -4.579669976578766785E-16, -5.898059818321121934E-17, -1.000000000000000000 ) ) ;
#7801 = EDGE_CURVE ( 'NONE', #605, #4429, #3884, .T. ) ;
#7802 = CARTESIAN_POINT ( 'NONE',  ( 7.999999999999563016, -4.618802153517398423, -7.685468820183672278 ) ) ;
#7803 = VERTEX_POINT ( 'NONE', #625 ) ;
#7804 = CYLINDRICAL_SURFACE ( 'NONE', #131, 5.000000000000034639 ) ;
#7805 = ORIENTED_EDGE ( 'NONE', *, *, #1294, .T. ) ;
#7806 = PRESENTATION_LAYER_ASSIGNMENT (  '', '', ( #2252 ) ) ;
#7807 = VECTOR ( 'NONE', #4776, 1000.000000000000114 ) ;
#7808 = CARTESIAN_POINT ( 'NONE',  ( -3.999999999999892530, 6.928203230275431501, 0.000000000000000000 ) ) ;
#7809 = ORIENTED_EDGE ( 'NONE', *, *, #3956, .T. ) ;
#7810 = EDGE_CURVE ( 'NONE', #4696, #6850, #5285, .T. ) ;
#7811 = VECTOR ( 'NONE', #5034, 1000.000000000000000 ) ;
#7812 = CARTESIAN_POINT ( 'NONE',  ( 0.000000000000000000, 0.000000000000000000, 0.000000000000000000 ) ) ;
#7813 =( NAMED_UNIT ( * ) SI_UNIT ( $, .STERADIAN. ) SOLID_ANGLE_UNIT ( ) );
#7814 = VECTOR ( 'NONE', #8017, 1000.000000000000000 ) ;
#7815 = CARTESIAN_POINT ( 'NONE',  ( -2.645508037661928213, -7.710219529346594491, -0.06809871960542769609 ) ) ;
#7816 = CYLINDRICAL_SURFACE ( 'NONE', #3183, 4.499999999999983125 ) ;
#7817 = DIRECTION ( 'NONE',  ( 1.000000000000000000, 2.775557561562898056E-15, -3.821045009664285041E-30 ) ) ;
#7818 = DIRECTION ( 'NONE',  ( 3.851859888774471706E-33, -7.598173571352216173E-18, 1.000000000000000000 ) ) ;
#7819 = VERTEX_POINT ( 'NONE', #4637 ) ;
#7820 = VERTEX_POINT ( 'NONE', #2674 ) ;
#7821 = DIRECTION ( 'NONE',  ( 2.842664852890546338E-35, -1.000000000000000000, 0.000000000000000000 ) ) ;
#7822 = CONICAL_SURFACE ( 'NONE', #6580, 75.00000000000005684, 0.7853981633974441712 ) ;
#7823 = CIRCLE ( 'NONE', #320, 4.499999999999997335 ) ;
#7824 = EDGE_CURVE ( 'NONE', #3235, #1504, #2451, .T. ) ;
#7825 = FACE_BOUND ( 'NONE', #2004, .T. ) ;
#7826 = CARTESIAN_POINT ( 'NONE',  ( 1.313474075707030897, 8.479269695850733868, -0.3167204509597497664 ) ) ;
#7827 = CONTEXT_DEPENDENT_SHAPE_REPRESENTATION ( #3229, #7451 ) ;
#7828 = EDGE_LOOP ( 'NONE', ( #8213, #7805, #8330, #4923, #1378, #8166 ) ) ;
#7829 = CARTESIAN_POINT ( 'NONE',  ( -49.99999999999944578, 152.5000000000003126, 9.999999999999786837 ) ) ;
#7830 = AXIS2_PLACEMENT_3D ( 'NONE', #3327, #1420, #1540 ) ;
#7831 = ORIENTED_EDGE ( 'NONE', *, *, #2191, .T. ) ;
#7832 = CYLINDRICAL_SURFACE ( 'NONE', #1052, 10.50000000000001066 ) ;
#7833 = VERTEX_POINT ( 'NONE', #575 ) ;
#7834 = EDGE_CURVE ( 'NONE', #5411, #4318, #2541, .T. ) ;
#7835 = CONICAL_SURFACE ( 'NONE', #331, 8.000000000000007105, 1.047197551196597631 ) ;
#7836 = CARTESIAN_POINT ( 'NONE',  ( 275.0000000000000000, -425.0000000000000000, 80.00000000000000000 ) ) ;
#7837 = LINE ( 'NONE', #7884, #88 ) ;
#7838 = PLANE ( 'NONE',  #3668 ) ;
#7839 = FACE_OUTER_BOUND ( 'NONE', #4572, .T. ) ;
#7840 = SURFACE_STYLE_FILL_AREA ( #5132 ) ;
#7841 = VERTEX_POINT ( 'NONE', #5197 ) ;
#7842 = AXIS2_PLACEMENT_3D ( 'NONE', #6861, #893, #3547 ) ;
#7843 = DIRECTION ( 'NONE',  ( 0.000000000000000000, 0.000000000000000000, 1.000000000000000000 ) ) ;
#7844 = ITEM_DEFINED_TRANSFORMATION ( 'NONE', 'NONE', #8402,  #7563 ) ;
#7845 = DIRECTION ( 'NONE',  ( -1.000000000000000000, -2.715219353702835870E-15, 0.000000000000000000 ) ) ;
#7846 = CYLINDRICAL_SURFACE ( 'NONE', #6683, 4.499999999999993783 ) ;
#7847 = ORIENTED_EDGE ( 'NONE', *, *, #2475, .F. ) ;
#7848 = CARTESIAN_POINT ( 'NONE',  ( 50.00000000000004263, -500.0000000000000000, -50.00000000000000000 ) ) ;
#7849 = ORIENTED_EDGE ( 'NONE', *, *, #2951, .F. ) ;
#7850 = ADVANCED_FACE ( 'NONE', ( #3232 ), #1323, .F. ) ;
#7851 = AXIS2_PLACEMENT_3D ( 'NONE', #1774, #3083, #4432 ) ;
#7852 = DIRECTION ( 'NONE',  ( -1.000000000000000000, 0.000000000000000000, 0.000000000000000000 ) ) ;
#7853 = PRODUCT ( 'hex nut style 1_am_B18.2.4.1M - Hex nut, Style 1,  M10 x 1.5, with 16mm WAF --D-N', 'hex nut style 1_am_B18.2.4.1M - Hex nut, Style 1,  M10 x 1.5, with 16mm WAF --D-N', '', ( #7032 ) ) ;
#7854 = VERTEX_POINT ( 'NONE', #5333 ) ;
#7855 = DIRECTION ( 'NONE',  ( -1.000000000000000000, 1.774937036747276562E-30, 0.000000000000000000 ) ) ;
#7856 = APPLICATION_CONTEXT ( 'automotive_design' ) ;
#7857 = PRODUCT_DEFINITION_CONTEXT ( 'detailed design', #3701, 'design' ) ;
#7858 = FACE_BOUND ( 'NONE', #459, .T. ) ;
#7859 = AXIS2_PLACEMENT_3D ( 'NONE', #6019, #5397, #14 ) ;
#7860 = FACE_OUTER_BOUND ( 'NONE', #3025, .T. ) ;
#7861 = DIRECTION ( 'NONE',  ( 0.000000000000000000, 0.000000000000000000, -1.000000000000000000 ) ) ;
#7862 = LINE ( 'NONE', #636, #6084 ) ;
#7863 = FACE_OUTER_BOUND ( 'NONE', #8180, .T. ) ;
#7864 = ORIENTED_EDGE ( 'NONE', *, *, #6043, .T. ) ;
#7865 = ADVANCED_FACE ( 'NONE', ( #7987, #2016, #4278 ), #4240, .F. ) ;
#7866 =( NAMED_UNIT ( * ) SI_UNIT ( $, .STERADIAN. ) SOLID_ANGLE_UNIT ( ) );
#7867 = VERTEX_POINT ( 'NONE', #1492 ) ;
#7868 = CARTESIAN_POINT ( 'NONE',  ( 0.000000000000000000, 295.0000000000000568, -6.938893903907228378E-14 ) ) ;
#7869 = CIRCLE ( 'NONE', #6906, 8.000000000000007105 ) ;
#7870 =( NAMED_UNIT ( * ) PLANE_ANGLE_UNIT ( ) SI_UNIT ( $, .RADIAN. ) );
#7871 = FACE_OUTER_BOUND ( 'NONE', #1667, .T. ) ;
#7872 = DIRECTION ( 'NONE',  ( -1.000000000000000000, -8.881784197001244435E-16, 0.000000000000000000 ) ) ;
#7873 = FACE_OUTER_BOUND ( 'NONE', #6253, .T. ) ;
#7874 = ORIENTED_EDGE ( 'NONE', *, *, #1345, .F. ) ;
#7875 = B_SPLINE_CURVE_WITH_KNOTS ( 'NONE', 3,
 ( #2578, #1220, #3876, #5187, #8452, #5135 ),
 .UNSPECIFIED., .F., .F.,
 ( 4, 2, 4 ),
 ( 2.380731628247754583E-07, 0.002336973833157303133, 0.004673709593151780146 ),
 .UNSPECIFIED. ) ;
#7876 = FACE_OUTER_BOUND ( 'NONE', #3560, .T. ) ;
#7877 = AXIS2_PLACEMENT_3D ( 'NONE', #507, #8309, #4342 ) ;
#7878 = EDGE_LOOP ( 'NONE', ( #7225, #1408, #2540, #258, #5516, #478 ) ) ;
#7879 = ADVANCED_FACE ( 'NONE', ( #6130 ), #2231, .F. ) ;
#7880 = ORIENTED_EDGE ( 'NONE', *, *, #1222, .T. ) ;
#7881 = CARTESIAN_POINT ( 'NONE',  ( -8.000000000000007105, -4.618802153517065356, -7.685468820183672278 ) ) ;
#7882 = FACE_OUTER_BOUND ( 'NONE', #1588, .T. ) ;
#7883 = VECTOR ( 'NONE', #8594, 1000.000000000000000 ) ;
#7884 = CARTESIAN_POINT ( 'NONE',  ( 5.000000000000004441, -2.342598717236951789, 4.057500000000047180 ) ) ;
#7885 = DIRECTION ( 'NONE',  ( 0.000000000000000000, -1.064348848528640545E-29, 1.000000000000000000 ) ) ;
#7886 = CARTESIAN_POINT ( 'NONE',  ( 8.000000000000234479, -1.555946510856281106, -0.06708870216350279470 ) ) ;
#7887 = SURFACE_SIDE_STYLE ('',( #8535 ) ) ;
#7888 = VERTEX_POINT ( 'NONE', #2929 ) ;
#7889 = EDGE_CURVE ( 'NONE', #7175, #2167, #5870, .T. ) ;
#7890 = CARTESIAN_POINT ( 'NONE',  ( 0.000000000000000000, -3.518949890710769690, 0.000000000000000000 ) ) ;
#7891 = EDGE_CURVE ( 'NONE', #2953, #1650, #5580, .T. ) ;
#7892 = PRODUCT_DEFINITION ( 'UNKNOWN', '', #3119, #2373 ) ;
#7893 = VECTOR ( 'NONE', #6231, 1000.000000000000114 ) ;
#7894 = CARTESIAN_POINT ( 'NONE',  ( 4.250000000000000888, 32.50000000000005684, -6.938893903907228378E-15 ) ) ;
#7895 = ORIENTED_EDGE ( 'NONE', *, *, #529, .F. ) ;
#7896 = DIRECTION ( 'NONE',  ( 0.000000000000000000, -1.213383262747659708E-29, 1.000000000000000000 ) ) ;
#7897 =( NAMED_UNIT ( * ) PLANE_ANGLE_UNIT ( ) SI_UNIT ( $, .RADIAN. ) );
#7898 = EDGE_LOOP ( 'NONE', ( #2564, #2162, #547, #3305 ) ) ;
#7899 = CARTESIAN_POINT ( 'NONE',  ( 3.318518101602789372, 7.321656987762753310, -8.400000000000137135 ) ) ;
#7900 = EDGE_LOOP ( 'NONE', ( #1625, #8515, #422, #2109 ) ) ;
#7901 = DIRECTION ( 'NONE',  ( 5.620633949699709114E-30, -0.8660254037844395958, -0.4999999999999983902 ) ) ;
#7902 = DIRECTION ( 'NONE',  ( 0.000000000000000000, 0.000000000000000000, 1.000000000000000000 ) ) ;
#7903 = CARTESIAN_POINT ( 'NONE',  ( -6.661338147750939243E-13, 9.237604307034352757, -8.400000000000018119 ) ) ;
#7904 = B_SPLINE_CURVE_WITH_KNOTS ( 'NONE', 3,
 ( #6659, #6107, #2778, #3905, #3958, #690 ),
 .UNSPECIFIED., .F., .F.,
 ( 4, 2, 4 ),
 ( 2.380731634700986265E-07, 0.002336973833157787988, 0.004673709593152105407 ),
 .UNSPECIFIED. ) ;
#7905 = DIRECTION ( 'NONE',  ( 0.000000000000000000, 0.000000000000000000, 1.000000000000000000 ) ) ;
#7906 = LINE ( 'NONE', #4652, #1299 ) ;
#7907 = ORIENTED_EDGE ( 'NONE', *, *, #4434, .T. ) ;
#7908 = VERTEX_POINT ( 'NONE', #182 ) ;
#7909 = CYLINDRICAL_SURFACE ( 'NONE', #4593, 25.00000000000000711 ) ;
#7910 = VECTOR ( 'NONE', #7713, 1000.000000000000114 ) ;
#7911 = B_SPLINE_CURVE_WITH_KNOTS ( 'NONE', 3,
 ( #5887, #8510, #7731, #5208, #7086, #1765 ),
 .UNSPECIFIED., .F., .F.,
 ( 4, 2, 4 ),
 ( 2.380731629388737080E-07, 0.002336973833157555101, 0.004673709593152171327 ),
 .UNSPECIFIED. ) ;
#7912 = DIRECTION ( 'NONE',  ( 0.000000000000000000, -1.064348848528640685E-29, 1.000000000000000000 ) ) ;
#7913 = ADVANCED_FACE ( 'NONE', ( #4931 ), #1943, .F. ) ;
#7914 = EDGE_LOOP ( 'NONE', ( #2566, #1547, #6327 ) ) ;
#7915 = TOROIDAL_SURFACE ( 'NONE', #8199, 4.400000000000030553, 0.4000000000000000222 ) ;
#7916 = DIRECTION ( 'NONE',  ( -3.919652622816902408E-30, -3.944304526105059027E-30, 1.000000000000000000 ) ) ;
#7917 = ORIENTED_EDGE ( 'NONE', *, *, #6751, .T. ) ;
#7918 = ORIENTED_EDGE ( 'NONE', *, *, #4938, .F. ) ;
#7919 = VECTOR ( 'NONE', #858, 1000.000000000000000 ) ;
#7920 = CARTESIAN_POINT ( 'NONE',  ( -4.000000000000003553, -6.928203230275431501, -8.400000000000018119 ) ) ;
#7921 = ORIENTED_EDGE ( 'NONE', *, *, #1926, .F. ) ;
#7922 = DIRECTION ( 'NONE',  ( 1.000000000000000000, -1.284024588418159550E-35, 3.851859888774464864E-33 ) ) ;
#7923 = VECTOR ( 'NONE', #8422, 1000.000000000000000 ) ;
#7924 = EDGE_CURVE ( 'NONE', #2093, #3646, #7589, .T. ) ;
#7925 = CARTESIAN_POINT ( 'NONE',  ( -34.99999999999963762, 120.0000000000003695, 5.879478934225333434E-29 ) ) ;
#7926 = CLOSED_SHELL ( 'NONE', ( #5166, #3225, #8580, #2071, #4588, #1110, #52, #8568, #4454, #3497, #6211, #7865, #5678, #6470, #3244, #6836, #696, #1672, #7879, #4728, #5120, #3920, #6272, #4925, #6010, #4410 ) ) ;
#7927 = EDGE_CURVE ( 'NONE', #3693, #662, #5513, .T. ) ;
#7928 = CARTESIAN_POINT ( 'NONE',  ( -99.99999999999958789, 120.0000000000001137, 0.000000000000000000 ) ) ;
#7929 =( LENGTH_UNIT ( ) NAMED_UNIT ( * ) SI_UNIT ( .MILLI., .METRE. ) );
#7930 = ORIENTED_EDGE ( 'NONE', *, *, #6201, .F. ) ;
#7931 = DIRECTION ( 'NONE',  ( 0.9237280213470678847, 0.3830490080632384942, 0.000000000000000000 ) ) ;
#7932 = VECTOR ( 'NONE', #4326, 1000.000000000000114 ) ;
#7933 = ITEM_DEFINED_TRANSFORMATION ( 'NONE', 'NONE', #4651,  #7563 ) ;
#7934 = EDGE_CURVE ( 'NONE', #8292, #2305, #6680, .T. ) ;
#7935 = CARTESIAN_POINT ( 'NONE',  ( 0.000000000000000000, -29.14213562373091548, -1.110223024625156540E-13 ) ) ;
#7936 = EDGE_CURVE ( 'NONE', #6954, #4437, #6148, .T. ) ;
#7937 = CIRCLE ( 'NONE', #2115, 4.057500000000000107 ) ;
#7938 = CARTESIAN_POINT ( 'NONE',  ( -9.999999999999884537, -14.99999999999990052, 79.99999999999995737 ) ) ;
#7939 = EDGE_LOOP ( 'NONE', ( #1956, #6036, #4204 ) ) ;
#7940 = DIRECTION ( 'NONE',  ( 7.703719777548943412E-34, 0.000000000000000000, -1.000000000000000000 ) ) ;
#7941 = DIRECTION ( 'NONE',  ( 1.463706757734299248E-32, -1.000000000000000000, -5.238529448733281520E-32 ) ) ;
#7942 = ORIENTED_EDGE ( 'NONE', *, *, #4325, .T. ) ;
#7943 = EDGE_CURVE ( 'NONE', #4252, #3370, #2921, .T. ) ;
#7944 = DIRECTION ( 'NONE',  ( -1.000000000000000000, -8.881784197001244435E-16, 0.000000000000000000 ) ) ;
#7945 = ORIENTED_EDGE ( 'NONE', *, *, #6877, .F. ) ;
#7946 = LINE ( 'NONE', #1978, #6193 ) ;
#7947 = B_SPLINE_CURVE_WITH_KNOTS ( 'NONE', 3,
 ( #8565, #6757, #7395, #6618, #8098, #2698 ),
 .UNSPECIFIED., .F., .F.,
 ( 4, 2, 4 ),
 ( 2.380731629386716377E-07, 0.002336973833157600638, 0.004673709593152262400 ),
 .UNSPECIFIED. ) ;
#7948 = CARTESIAN_POINT ( 'NONE',  ( -6.661338147750939243E-13, -9.237604307034352757, -7.685468820183672278 ) ) ;
#7949 = CYLINDRICAL_SURFACE ( 'NONE', #8063, 5.749999999999991118 ) ;
#7950 = LINE ( 'NONE', #3332, #6040 ) ;
#7951 = DIRECTION ( 'NONE',  ( 3.549874073494553825E-30, -1.000000000000000000, 1.478898702612476446E-15 ) ) ;
#7952 = VECTOR ( 'NONE', #2592, 1000.000000000000000 ) ;
#7953 = FACE_OUTER_BOUND ( 'NONE', #7914, .T. ) ;
#7954 = ORIENTED_EDGE ( 'NONE', *, *, #3690, .F. ) ;
#7955 = DIRECTION ( 'NONE',  ( 0.000000000000000000, -4.930380657631321594E-32, -1.000000000000000000 ) ) ;
#7956 = ORIENTED_EDGE ( 'NONE', *, *, #6119, .T. ) ;
#7957 = DIRECTION ( 'NONE',  ( 0.000000000000000000, -5.322451846059955323E-30, 1.000000000000000000 ) ) ;
#7958 = AXIS2_PLACEMENT_3D ( 'NONE', #1194, #6472, #3162 ) ;
#7959 = UNCERTAINTY_MEASURE_WITH_UNIT (LENGTH_MEASURE( 1.000000000000000082E-05 ), #7490, 'distance_accuracy_value', 'NONE');
#7960 = SURFACE_SIDE_STYLE ('',( #5896 ) ) ;
#7961 = DIRECTION ( 'NONE',  ( -1.000000000000000000, 3.549874073494553124E-30, 0.000000000000000000 ) ) ;
#7962 = CONTEXT_DEPENDENT_SHAPE_REPRESENTATION ( #104, #5008 ) ;
#7963 = AXIS2_PLACEMENT_3D ( 'NONE', #3598, #4816, #4727 ) ;
#7964 = CARTESIAN_POINT ( 'NONE',  ( -5.080504117408895404, -2.106769544347820933, -8.401000000000047763 ) ) ;
#7965 = DIRECTION ( 'NONE',  ( 0.000000000000000000, 0.000000000000000000, 1.000000000000000000 ) ) ;
#7966 = VERTEX_POINT ( 'NONE', #2117 ) ;
#7967 = CARTESIAN_POINT ( 'NONE',  ( -7.999999999999890754, -1.555946510856244025, -0.06708870216330432845 ) ) ;
#7968 = ORIENTED_EDGE ( 'NONE', *, *, #7889, .T. ) ;
#7969 = EDGE_CURVE ( 'NONE', #6439, #3947, #6278, .T. ) ;
#7970 = DIRECTION ( 'NONE',  ( 1.000000000000000000, 0.000000000000000000, 0.000000000000000000 ) ) ;
#7971 = EDGE_LOOP ( 'NONE', ( #3804, #3082, #2586, #3523 ) ) ;
#7972 = CARTESIAN_POINT ( 'NONE',  ( 0.000000000000000000, 0.000000000000000000, -8.400000000000018119 ) ) ;
#7973 = CARTESIAN_POINT ( 'NONE',  ( 8.000000000000229150, -1.665334536937734811E-13, 0.000000000000000000 ) ) ;
#7974 = DIRECTION ( 'NONE',  ( 1.000000000000000000, 8.881784197001244435E-16, 0.000000000000000000 ) ) ;
#7975 = AXIS2_PLACEMENT_3D ( 'NONE', #3970, #1405, #4759 ) ;
#7976 = AXIS2_PLACEMENT_3D ( 'NONE', #76, #5320, #7974 ) ;
#7977 = FACE_OUTER_BOUND ( 'NONE', #2829, .T. ) ;
#7978 = CARTESIAN_POINT ( 'NONE',  ( 0.000000000000000000, -2.342598717236902939, 4.057500000000047180 ) ) ;
#7979 = ORIENTED_EDGE ( 'NONE', *, *, #6448, .T. ) ;
#7980 = ORIENTED_EDGE ( 'NONE', *, *, #7102, .T. ) ;
#7981 = AXIS2_PLACEMENT_3D ( 'NONE', #8090, #816, #3428 ) ;
#7982 = APPLICATION_PROTOCOL_DEFINITION ( 'draft international standard', 'automotive_design', 1998, #3239 ) ;
#7983 = ADVANCED_FACE ( 'NONE', ( #1452 ), #889, .F. ) ;
#7984 = DIRECTION ( 'NONE',  ( 3.851859888774471706E-33, -7.598173571352223877E-18, 1.000000000000000000 ) ) ;
#7985 = CONICAL_SURFACE ( 'NONE', #168, 8.000000000000007105, 1.047197551196597631 ) ;
#7986 = ORIENTED_EDGE ( 'NONE', *, *, #1124, .F. ) ;
#7987 = FACE_BOUND ( 'NONE', #512, .T. ) ;
#7988 = DIRECTION ( 'NONE',  ( -1.000000000000000000, 1.774937036747276562E-30, 0.000000000000000000 ) ) ;
#7989 =( LENGTH_UNIT ( ) NAMED_UNIT ( * ) SI_UNIT ( .MILLI., .METRE. ) );
#7990 = ORIENTED_EDGE ( 'NONE', *, *, #3254, .F. ) ;
#7991 = AXIS2_PLACEMENT_3D ( 'NONE', #6779, #6820, #802 ) ;
#7992 = EDGE_CURVE ( 'NONE', #7037, #6198, #8481, .T. ) ;
#7993 = CARTESIAN_POINT ( 'NONE',  ( 4.339467034331171646, 6.732211846623375351, -8.400000000000034106 ) ) ;
#7994 = ORIENTED_EDGE ( 'NONE', *, *, #7230, .F. ) ;
#7995 = CARTESIAN_POINT ( 'NONE',  ( -5.355005115540977911, -6.145890662064671162, -0.08224679563975283159 ) ) ;
#7996 = DIRECTION ( 'NONE',  ( 0.000000000000000000, 0.000000000000000000, -1.000000000000000000 ) ) ;
#7997 = LINE ( 'NONE', #1284, #6029 ) ;
#7998 = DIRECTION ( 'NONE',  ( 1.000000000000000000, -3.549874073494553124E-30, 0.000000000000000000 ) ) ;
#7999 = DIRECTION ( 'NONE',  ( 0.8660254037844367092, -0.5000000000000033307, 0.000000000000000000 ) ) ;
#8000 = LINE ( 'NONE', #7301, #5193 ) ;
#8001 = EDGE_LOOP ( 'NONE', ( #117, #1732, #6346, #4955 ) ) ;
#8002 = LINE ( 'NONE', #4654, #7378 ) ;
#8003 = PRESENTATION_STYLE_ASSIGNMENT (( #4739 ) ) ;
#8004 = DIRECTION ( 'NONE',  ( -1.000000000000000000, -8.881784197001244435E-16, 0.000000000000000000 ) ) ;
#8005 = CARTESIAN_POINT ( 'NONE',  ( -77.99999999999941735, 120.0000000000003411, -2.775557561562889458E-14 ) ) ;
#8006 = DIRECTION ( 'NONE',  ( 1.000000000000000000, 8.881784197001244435E-16, 0.000000000000000000 ) ) ;
#8007 = DIRECTION ( 'NONE',  ( 6.400024471207000214E-36, -1.000000000000000000, 0.000000000000000000 ) ) ;
#8008 = EDGE_CURVE ( 'NONE', #6142, #5854, #7363, .T. ) ;
#8009 = EDGE_CURVE ( 'NONE', #1219, #872, #6859, .T. ) ;
#8010 = PLANE ( 'NONE',  #1512 ) ;
#8011 = DIRECTION ( 'NONE',  ( 0.000000000000000000, 0.000000000000000000, 1.000000000000000000 ) ) ;
#8012 = ORIENTED_EDGE ( 'NONE', *, *, #1993, .F. ) ;
#8013 = B_SPLINE_CURVE_WITH_KNOTS ( 'NONE', 3,
 ( #1246, #2652, #6616, #5448, #604, #7348 ),
 .UNSPECIFIED., .F., .F.,
 ( 4, 2, 4 ),
 ( 0.01291313371729461111, 0.01525081363757312125, 0.01758849355785162966 ),
 .UNSPECIFIED. ) ;
#8014 = CIRCLE ( 'NONE', #4113, 14.99999999999987388 ) ;
#8015 = CARTESIAN_POINT ( 'NONE',  ( -8.000000000000007105, -4.618802153517065356, -0.7145311798163467287 ) ) ;
#8016 = ORIENTED_EDGE ( 'NONE', *, *, #4717, .F. ) ;
#8017 = DIRECTION ( 'NONE',  ( -3.851859888774471706E-33, -1.232595164407830946E-32, -1.000000000000000000 ) ) ;
#8018 = EDGE_LOOP ( 'NONE', ( #6777, #2238, #1977, #333, #5021 ) ) ;
#8019 = LINE ( 'NONE', #2049, #8126 ) ;
#8020 = DIRECTION ( 'NONE',  ( -1.000000000000000000, -3.083952846180994816E-15, 0.000000000000000000 ) ) ;
#8021 = DIRECTION ( 'NONE',  ( -0.000000000000000000, -1.000000000000000000, -0.000000000000000000 ) ) ;
#8022 = EDGE_CURVE ( 'NONE', #3886, #749, #8201, .T. ) ;
#8023 = CARTESIAN_POINT ( 'NONE',  ( 0.000000000000000000, 0.000000000000000000, -8.400000000000018119 ) ) ;
#8024 = DIRECTION ( 'NONE',  ( -1.000000000000000000, 3.549874073494553124E-30, 0.000000000000000000 ) ) ;
#8025 = PRODUCT_RELATED_PRODUCT_CATEGORY ( 'part', '', ( #552 ) ) ;
#8026 = ORIENTED_EDGE ( 'NONE', *, *, #7198, .F. ) ;
#8027 = VERTEX_POINT ( 'NONE', #1785 ) ;
#8028 = AXIS2_PLACEMENT_3D ( 'NONE', #346, #7013, #1554 ) ;
#8029 = DIRECTION ( 'NONE',  ( -1.000000000000000000, 3.549874073494553124E-30, 3.778304382545602261E-59 ) ) ;
#8030 = EDGE_CURVE ( 'NONE', #5152, #4437, #5827, .T. ) ;
#8031 = ORIENTED_EDGE ( 'NONE', *, *, #2250, .F. ) ;
#8032 = CARTESIAN_POINT ( 'NONE',  ( 8.000000000000117240, 4.618802153517009401, -7.685468820183672278 ) ) ;
#8033 = AXIS2_PLACEMENT_3D ( 'NONE', #4559, #4039, #687 ) ;
#8034 = DIRECTION ( 'NONE',  ( 1.000000000000000000, 0.000000000000000000, 0.000000000000000000 ) ) ;
#8035 = ORIENTED_EDGE ( 'NONE', *, *, #6074, .F. ) ;
#8036 = CARTESIAN_POINT ( 'NONE',  ( 6.123233995736764507E-15, 49.99999999999999289, -10.00000000000006395 ) ) ;
#8037 = ORIENTED_EDGE ( 'NONE', *, *, #3041, .T. ) ;
#8038 = CARTESIAN_POINT ( 'NONE',  ( 28.24999999999996803, 1.387778780781445676E-14, 18.00000000000000355 ) ) ;
#8039 = CARTESIAN_POINT ( 'NONE',  ( 0.000000000000000000, 0.000000000000000000, 0.000000000000000000 ) ) ;
#8040 = EDGE_CURVE ( 'NONE', #3237, #3424, #1651, .T. ) ;
#8041 = CYLINDRICAL_SURFACE ( 'NONE', #2383, 50.00000000000008527 ) ;
#8042 = DIRECTION ( 'NONE',  ( 3.851859888774471706E-33, -7.598173571352223877E-18, 1.000000000000000000 ) ) ;
#8043 = CARTESIAN_POINT ( 'NONE',  ( -1.310872448937907997, 8.480771745766357839, -0.3173508448886235289 ) ) ;
#8044 = VERTEX_POINT ( 'NONE', #8420 ) ;
#8045 = CARTESIAN_POINT ( 'NONE',  ( -7.999999999999894307, 1.572549600175511042, -0.06894455525505825688 ) ) ;
#8046 = CARTESIAN_POINT ( 'NONE',  ( 0.000000000000000000, -9.237604307034075646, -0.7145311798163467287 ) ) ;
#8047 = EDGE_CURVE ( 'NONE', #363, #6269, #1035, .T. ) ;
#8048 = EDGE_CURVE ( 'NONE', #2093, #4094, #431, .T. ) ;
#8049 = CARTESIAN_POINT ( 'NONE',  ( 9.184850993605148733E-15, -294.9999999999998295, -75.00000000000005684 ) ) ;
#8050 = FACE_OUTER_BOUND ( 'NONE', #4705, .T. ) ;
#8051 = ORIENTED_EDGE ( 'NONE', *, *, #943, .F. ) ;
#8052 = CIRCLE ( 'NONE', #279, 10.50000000000001066 ) ;
#8053 = ORIENTED_EDGE ( 'NONE', *, *, #7291, .T. ) ;
#8054 = FACE_BOUND ( 'NONE', #3908, .T. ) ;
#8055 = VERTEX_POINT ( 'NONE', #5012 ) ;
#8056 = DIRECTION ( 'NONE',  ( 1.000000000000000000, -0.000000000000000000, -6.938893903907228378E-17 ) ) ;
#8057 = EDGE_CURVE ( 'NONE', #748, #6735, #5138, .T. ) ;
#8058 = CIRCLE ( 'NONE', #407, 49.99999999999998579 ) ;
#8059 = CARTESIAN_POINT ( 'NONE',  ( -8.000000000000222045, -3.098204225878416818, -8.084209322807978992 ) ) ;
#8060 = VECTOR ( 'NONE', #2441, 1000.000000000000000 ) ;
#8061 = CIRCLE ( 'NONE', #8193, 15.00000000000000355 ) ;
#8062 = CARTESIAN_POINT ( 'NONE',  ( 0.000000000000000000, -9.237604307034075646, -0.7145311798163467287 ) ) ;
#8063 = AXIS2_PLACEMENT_3D ( 'NONE', #5298, #6012, #6603 ) ;
#8064 = ORIENTED_EDGE ( 'NONE', *, *, #3590, .T. ) ;
#8065 = EDGE_LOOP ( 'NONE', ( #1485, #4609, #2181, #8261 ) ) ;
#8066 = CIRCLE ( 'NONE', #5277, 5.500000000000000000 ) ;
#8067 = CLOSED_SHELL ( 'NONE', ( #4702, #4114, #5040, #1080, #2875, #5511, #6541, #2725, #4073, #2596, #536, #8131, #5019, #5982, #5396, #4595, #7182, #5391, #5897, #4327, #3264, #2208 ) ) ;
#8068 = EDGE_CURVE ( 'NONE', #3237, #8125, #689, .T. ) ;
#8069 = CONICAL_SURFACE ( 'NONE', #5998, 4.171999999999999709, 0.7853981633975604115 ) ;
#8070 = VECTOR ( 'NONE', #8460, 1000.000000000000000 ) ;
#8071 = DIRECTION ( 'NONE',  ( 0.000000000000000000, 0.000000000000000000, -1.000000000000000000 ) ) ;
#8072 = ORIENTED_EDGE ( 'NONE', *, *, #2672, .T. ) ;
#8073 = AXIS2_PLACEMENT_3D ( 'NONE', #8379, #5146, #5830 ) ;
#8074 = MECHANICAL_DESIGN_GEOMETRIC_PRESENTATION_REPRESENTATION (  '', ( #8211 ), #8487 ) ;
#8075 = CARTESIAN_POINT ( 'NONE',  ( -34.92499999999998295, 0.000000000000000000, 10.00000000000000178 ) ) ;
#8076 = VECTOR ( 'NONE', #6203, 1000.000000000000000 ) ;
#8077 = DIRECTION ( 'NONE',  ( 0.000000000000000000, 0.000000000000000000, 1.000000000000000000 ) ) ;
#8078 = ORIENTED_EDGE ( 'NONE', *, *, #5341, .F. ) ;
#8079 = AXIS2_PLACEMENT_3D ( 'NONE', #2215, #6977, #4308 ) ;
#8080 = DIRECTION ( 'NONE',  ( -3.851859888774471706E-33, -1.232595164407830946E-32, -1.000000000000000000 ) ) ;
#8081 = PRODUCT_DEFINITION_SHAPE ( 'NONE', 'NONE',  #8617 ) ;
#8082 = ORIENTED_EDGE ( 'NONE', *, *, #5859, .T. ) ;
#8083 = DIRECTION ( 'NONE',  ( 1.540743955509788682E-33, 4.592425496802573602E-17, -1.000000000000000000 ) ) ;
#8084 = ADVANCED_FACE ( 'NONE', ( #8374 ), #7771, .T. ) ;
#8085 = CARTESIAN_POINT ( 'NONE',  ( 38.74999999999999289, 4.745506346695993302E-15, 18.00000000000000355 ) ) ;
#8086 = EDGE_LOOP ( 'NONE', ( #783, #7994, #3978 ) ) ;
#8087 = CARTESIAN_POINT ( 'NONE',  ( -44.99999999999992895, -500.0000000000000000, -45.00000000000000711 ) ) ;
#8088 = CARTESIAN_POINT ( 'NONE',  ( 6.123233995736776340E-15, 50.00000000000008527, -109.9999999999999574 ) ) ;
#8089 = CARTESIAN_POINT ( 'NONE',  ( -2.644994884459048290, 7.710515798486305528, -0.08224679563966873219 ) ) ;
#8090 = CARTESIAN_POINT ( 'NONE',  ( -50.00000000000004263, 425.0000000000000000, 3.469446951953614189E-15 ) ) ;
#8091 = ORIENTED_EDGE ( 'NONE', *, *, #4763, .F. ) ;
#8092 = VECTOR ( 'NONE', #3874, 1000.000000000000000 ) ;
#8093 = DIRECTION ( 'NONE',  ( 1.885870601543981347E-30, -1.000000000000000000, 7.405124331421681105E-16 ) ) ;
#8094 = VERTEX_POINT ( 'NONE', #313 ) ;
#8095 = EDGE_CURVE ( 'NONE', #3003, #7090, #3012, .T. ) ;
#8096 = ADVANCED_FACE ( 'NONE', ( #7631 ), #2657, .T. ) ;
#8097 = CARTESIAN_POINT ( 'NONE',  ( -275.0000000000000000, -425.0000000000000000, 80.00000000000000000 ) ) ;
#8098 = CARTESIAN_POINT ( 'NONE',  ( 4.681481898397022334, -6.534749472788251801, -5.280064580004406594E-14 ) ) ;
#8099 = DIRECTION ( 'NONE',  ( 1.000000000000000000, 3.083952846180992055E-15, 0.000000000000000000 ) ) ;
#8100 = VERTEX_POINT ( 'NONE', #496 ) ;
#8101 = CARTESIAN_POINT ( 'NONE',  ( 5.551115123125782702E-14, -2.342598717236909600, -4.057500000000047180 ) ) ;
#8102 = ORIENTED_EDGE ( 'NONE', *, *, #4982, .T. ) ;
#8103 = AXIS2_PLACEMENT_3D ( 'NONE', #1552, #6838, #5676 ) ;
#8104 = EDGE_CURVE ( 'NONE', #4193, #367, #3331, .T. ) ;
#8105 = DIRECTION ( 'NONE',  ( 0.000000000000000000, 0.000000000000000000, 1.000000000000000000 ) ) ;
#8106 = VECTOR ( 'NONE', #2272, 1000.000000000000114 ) ;
#8107 = AXIS2_PLACEMENT_3D ( 'NONE', #7564, #2943, #4293 ) ;
#8108 = CARTESIAN_POINT ( 'NONE',  ( 0.000000000000000000, 0.000000000000000000, -8.400000000000018119 ) ) ;
#8109 = DIRECTION ( 'NONE',  ( -2.728201748236247839E-33, 0.7071067811865454633, -0.7071067811865495711 ) ) ;
#8110 = EDGE_LOOP ( 'NONE', ( #7765, #1913, #6978, #6482, #8527, #2669 ) ) ;
#8111 = DIRECTION ( 'NONE',  ( 3.851859888774471706E-33, -7.598173571352223877E-18, 1.000000000000000000 ) ) ;
#8112 = EDGE_LOOP ( 'NONE', ( #4099, #2225 ) ) ;
#8113 = ORIENTED_EDGE ( 'NONE', *, *, #222, .F. ) ;
#8114 = VECTOR ( 'NONE', #5184, 1000.000000000000000 ) ;
#8115 = VECTOR ( 'NONE', #7485, 1000.000000000000000 ) ;
#8116 = CARTESIAN_POINT ( 'NONE',  ( 0.000000000000000000, 0.000000000000000000, 0.000000000000000000 ) ) ;
#8117 = CARTESIAN_POINT ( 'NONE',  ( 8.000000000000007105, 4.618802153516899267, -7.685468820183672278 ) ) ;
#8118 = EDGE_LOOP ( 'NONE', ( #1256, #2234, #4458 ) ) ;
#8119 = ADVANCED_FACE ( 'NONE', ( #974 ), #2973, .T. ) ;
#8120 = CARTESIAN_POINT ( 'NONE',  ( -82.49999999999945999, 120.0000000000003268, 10.00000000000000888 ) ) ;
#8121 = AXIS2_PLACEMENT_3D ( 'NONE', #1051, #3823, #6519 ) ;
#8122 = FACE_OUTER_BOUND ( 'NONE', #5100, .T. ) ;
#8123 = DIRECTION ( 'NONE',  ( -4.579669976578770729E-16, -5.898059818321084956E-17, -1.000000000000000000 ) ) ;
#8124 = ORIENTED_EDGE ( 'NONE', *, *, #3401, .T. ) ;
#8125 = VERTEX_POINT ( 'NONE', #2351 ) ;
#8126 = VECTOR ( 'NONE', #7356, 1000.000000000000000 ) ;
#8127 = FACE_OUTER_BOUND ( 'NONE', #1706, .T. ) ;
#8128 = CARTESIAN_POINT ( 'NONE',  ( -44.99999999999992895, 500.0000000000000000, 50.00000000000000000 ) ) ;
#8129 = EDGE_LOOP ( 'NONE', ( #4835, #5024, #915, #5244 ) ) ;
#8130 = CARTESIAN_POINT ( 'NONE',  ( 4.000000000000003553, 6.938893903907228378E-14, 3.047499999999869758 ) ) ;
#8131 = ADVANCED_FACE ( 'NONE', ( #6382 ), #1541, .T. ) ;
#8132 = AXIS2_PLACEMENT_3D ( 'NONE', #4933, #6302, #228 ) ;
#8133 = VERTEX_POINT ( 'NONE', #451 ) ;
#8134 = FACE_BOUND ( 'NONE', #5714, .T. ) ;
#8135 =( NAMED_UNIT ( * ) SI_UNIT ( $, .STERADIAN. ) SOLID_ANGLE_UNIT ( ) );
#8136 = PRODUCT_DEFINITION_FORMATION_WITH_SPECIFIED_SOURCE ( 'ANY', '', #5939, .NOT_KNOWN. ) ;
#8137 = DIRECTION ( 'NONE',  ( -3.851859888774471706E-33, -1.232595164407830946E-32, -1.000000000000000000 ) ) ;
#8138 = CARTESIAN_POINT ( 'NONE',  ( -49.99999999999953815, 120.0000000000003268, 9.999999999999980460 ) ) ;
#8139 = CARTESIAN_POINT ( 'NONE',  ( 7.345652830558768720, -4.996589667937484158, -7.903584543331182211 ) ) ;
#8140 = EDGE_CURVE ( 'NONE', #650, #3046, #5015, .T. ) ;
#8141 = AXIS2_PLACEMENT_3D ( 'NONE', #1821, #6410, #444 ) ;
#8142 = CARTESIAN_POINT ( 'NONE',  ( 5.000000000000004441, -2.342598717236951789, 4.057500000000047180 ) ) ;
#8143 = ORIENTED_EDGE ( 'NONE', *, *, #3792, .F. ) ;
#8144 = SURFACE_STYLE_USAGE ( .BOTH. , #737 ) ;
#8145 = EDGE_LOOP ( 'NONE', ( #5199, #6409 ) ) ;
#8146 = DIRECTION ( 'NONE',  ( -0.000000000000000000, -0.000000000000000000, 1.000000000000000000 ) ) ;
#8147 = CARTESIAN_POINT ( 'NONE',  ( 5.000000000000004441, 4.685197434473897360, 0.000000000000000000 ) ) ;
#8148 = DIRECTION ( 'NONE',  ( 1.000000000000000000, 8.881784197001244435E-16, 0.000000000000000000 ) ) ;
#8149 = DIRECTION ( 'NONE',  ( -3.851859888774471706E-33, -1.232595164407830946E-32, -1.000000000000000000 ) ) ;
#8150 = VERTEX_POINT ( 'NONE', #1061 ) ;
#8151 = FACE_OUTER_BOUND ( 'NONE', #2543, .T. ) ;
#8152 = ORIENTED_EDGE ( 'NONE', *, *, #4857, .T. ) ;
#8153 = EDGE_CURVE ( 'NONE', #5405, #2192, #7480, .T. ) ;
#8154 = ORIENTED_EDGE ( 'NONE', *, *, #8307, .T. ) ;
#8155 = SURFACE_SIDE_STYLE ('',( #5460 ) ) ;
#8156 = DIRECTION ( 'NONE',  ( 0.000000000000000000, 5.322451846059958826E-30, -1.000000000000000000 ) ) ;
#8157 = ADVANCED_FACE ( 'NONE', ( #6619 ), #4131, .F. ) ;
#8158 = VERTEX_POINT ( 'NONE', #112 ) ;
#8159 = ADVANCED_FACE ( 'NONE', ( #1346 ), #1475, .F. ) ;
#8160 = CARTESIAN_POINT ( 'NONE',  ( -3.319543390095988755, 7.321065037175355172, -8.383111142572301944 ) ) ;
#8161 = CIRCLE ( 'NONE', #1900, 24.50000000000000000 ) ;
#8162 = DIRECTION ( 'NONE',  ( 0.000000000000000000, -1.000000000000000000, -1.795949010423047374E-16 ) ) ;
#8163 = DIRECTION ( 'NONE',  ( 0.000000000000000000, 0.000000000000000000, -1.000000000000000000 ) ) ;
#8164 = VERTEX_POINT ( 'NONE', #67 ) ;
#8165 = CARTESIAN_POINT ( 'NONE',  ( 50.00000000000004263, -425.0000000000000000, -3.469446951953614189E-15 ) ) ;
#8166 = ORIENTED_EDGE ( 'NONE', *, *, #4272, .F. ) ;
#8167 = CARTESIAN_POINT ( 'NONE',  ( 5.000000000000060396, -3.513898075855427461, -2.028750000000023590 ) ) ;
#8168 = DIRECTION ( 'NONE',  ( 0.000000000000000000, 0.000000000000000000, 1.000000000000000000 ) ) ;
#8169 = ORIENTED_EDGE ( 'NONE', *, *, #3516, .F. ) ;
#8170 = AXIS2_PLACEMENT_3D ( 'NONE', #614, #2612, #2478 ) ;
#8171 = CARTESIAN_POINT ( 'NONE',  ( -1.989930189099410700E-33, 9.499999999999976907, 130.0000000000000000 ) ) ;
#8172 = FACE_OUTER_BOUND ( 'NONE', #5653, .T. ) ;
#8173 = ORIENTED_EDGE ( 'NONE', *, *, #165, .T. ) ;
#8174 = ORIENTED_EDGE ( 'NONE', *, *, #177, .F. ) ;
#8175 = DIRECTION ( 'NONE',  ( 0.000000000000000000, 0.000000000000000000, 1.000000000000000000 ) ) ;
#8176 = CARTESIAN_POINT ( 'NONE',  ( 0.6527133886625599013, -8.860760056385744932, -0.4969600502617356197 ) ) ;
#8177 = DIRECTION ( 'NONE',  ( 6.400024471207000214E-36, -1.000000000000000000, 0.000000000000000000 ) ) ;
#8178 = DIRECTION ( 'NONE',  ( -1.000000000000000000, 0.000000000000000000, 0.000000000000000000 ) ) ;
#8179 = CARTESIAN_POINT ( 'NONE',  ( -275.0000000000000000, -425.0000000000000000, 80.00000000000000000 ) ) ;
#8180 = EDGE_LOOP ( 'NONE', ( #3536, #6688, #1349, #1248 ) ) ;
#8181 = DIRECTION ( 'NONE',  ( 0.000000000000000000, 0.8660254037844394848, 0.4999999999999986122 ) ) ;
#8182 = ORIENTED_EDGE ( 'NONE', *, *, #7414, .T. ) ;
#8183 = CYLINDRICAL_SURFACE ( 'NONE', #4202, 5.500000000000000000 ) ;
#8184 = EDGE_CURVE ( 'NONE', #5417, #1391, #3822, .T. ) ;
#8185 = CARTESIAN_POINT ( 'NONE',  ( -31.74999999999994316, -1.972152263052529514E-28, 0.000000000000000000 ) ) ;
#8186 = ORIENTED_EDGE ( 'NONE', *, *, #710, .F. ) ;
#8187 = DIRECTION ( 'NONE',  ( 0.000000000000000000, 0.000000000000000000, 1.000000000000000000 ) ) ;
#8188 = ORIENTED_EDGE ( 'NONE', *, *, #1015, .T. ) ;
#8189 = ORIENTED_EDGE ( 'NONE', *, *, #5793, .F. ) ;
#8190 = APPLICATION_CONTEXT ( 'automotive_design' ) ;
#8191 = AXIS2_PLACEMENT_3D ( 'NONE', #5734, #8443, #8364 ) ;
#8192 = EDGE_CURVE ( 'NONE', #6699, #8150, #3478, .T. ) ;
#8193 = AXIS2_PLACEMENT_3D ( 'NONE', #4335, #499, #6461 ) ;
#8194 = LINE ( 'NONE', #260, #1297 ) ;
#8195 = CYLINDRICAL_SURFACE ( 'NONE', #4453, 15.00000000000000355 ) ;
#8196 = ORIENTED_EDGE ( 'NONE', *, *, #1644, .F. ) ;
#8197 = CIRCLE ( 'NONE', #7207, 4.057500000000000107 ) ;
#8198 = VECTOR ( 'NONE', #2222, 1000.000000000000000 ) ;
#8199 = AXIS2_PLACEMENT_3D ( 'NONE', #5299, #7998, #3426 ) ;
#8200 = AXIS2_PLACEMENT_3D ( 'NONE', #1788, #2404, #3301 ) ;
#8201 = LINE ( 'NONE', #4887, #6831 ) ;
#8202 = CARTESIAN_POINT ( 'NONE',  ( -275.0000000000000000, 425.0000000000000000, -79.99999999999984368 ) ) ;
#8203 = CARTESIAN_POINT ( 'NONE',  ( 487.5000000000001705, 29.99999999999836220, 67.99999999999991473 ) ) ;
#8204 = ORIENTED_EDGE ( 'NONE', *, *, #2051, .F. ) ;
#8205 = DIRECTION ( 'NONE',  ( 3.851859888774471706E-33, 1.232595164407830946E-32, 1.000000000000000000 ) ) ;
#8206 = AXIS2_PLACEMENT_3D ( 'NONE', #1655, #6949, #8333 ) ;
#8207 = ORIENTED_EDGE ( 'NONE', *, *, #2527, .F. ) ;
#8208 = CARTESIAN_POINT ( 'NONE',  ( 275.0000000000000000, 425.0000000000000000, 1.561424668912875158E-13 ) ) ;
#8209 = EDGE_CURVE ( 'NONE', #7222, #4804, #2289, .T. ) ;
#8210 = CARTESIAN_POINT ( 'NONE',  ( 6.720025694767387310E-35, -10.50000000000001421, 128.9999999999999432 ) ) ;
#8211=STYLED_ITEM('',(#8670),#40);
#8212 = DIRECTION ( 'NONE',  ( -6.400024471207028278E-36, 1.000000000000000000, 0.000000000000000000 ) ) ;
#8213 = ORIENTED_EDGE ( 'NONE', *, *, #2683, .T. ) ;
#8214 = VECTOR ( 'NONE', #328, 1000.000000000000000 ) ;
#8215 = PLANE ( 'NONE',  #2498 ) ;
#8216 = CARTESIAN_POINT ( 'NONE',  ( -2.645508037661968181, -7.710219529346637124, -8.331901280394562903 ) ) ;
#8217 = ORIENTED_EDGE ( 'NONE', *, *, #2537, .T. ) ;
#8218 = PRESENTATION_LAYER_ASSIGNMENT (  '', '', ( #2229 ) ) ;
#8219 = EDGE_CURVE ( 'NONE', #8133, #3409, #4091, .T. ) ;
#8220 = DIRECTION ( 'NONE',  ( -3.851859888774471706E-33, -1.232595164407830946E-32, -1.000000000000000000 ) ) ;
#8221 = ORIENTED_EDGE ( 'NONE', *, *, #5752, .T. ) ;
#8222 = ORIENTED_EDGE ( 'NONE', *, *, #8040, .F. ) ;
#8223 = VECTOR ( 'NONE', #7770, 1000.000000000000000 ) ;
#8224 = PRODUCT_DEFINITION_CONTEXT ( 'detailed design', #6817, 'design' ) ;
#8225 = FACE_OUTER_BOUND ( 'NONE', #5246, .T. ) ;
#8226 = CARTESIAN_POINT ( 'NONE',  ( 9.999999999999896971, 0.000000000000000000, 0.000000000000000000 ) ) ;
#8227 = DIRECTION ( 'NONE',  ( 0.000000000000000000, 0.000000000000000000, 1.000000000000000000 ) ) ;
#8228 = CARTESIAN_POINT ( 'NONE',  ( 4.681481898397022334, -6.534749472788251801, -8.399999999999964828 ) ) ;
#8229 = CARTESIAN_POINT ( 'NONE',  ( -79.99999999999980105, 15.00000000000012434, 10.00000000000017586 ) ) ;
#8230 = ORIENTED_EDGE ( 'NONE', *, *, #632, .F. ) ;
#8231 = EDGE_CURVE ( 'NONE', #8316, #181, #201, .T. ) ;
#8232 = DIRECTION ( 'NONE',  ( 3.851859888774471706E-33, 1.232595164407830946E-32, 1.000000000000000000 ) ) ;
#8233 = ORIENTED_EDGE ( 'NONE', *, *, #3929, .F. ) ;
#8234 = VECTOR ( 'NONE', #5993, 1000.000000000000000 ) ;
#8235 = AXIS2_PLACEMENT_3D ( 'NONE', #3033, #5760, #5720 ) ;
#8236 = CARTESIAN_POINT ( 'NONE',  ( 0.000000000000000000, 6.809036203259282560E-16, -5.559999999999998721 ) ) ;
#8237 = DIRECTION ( 'NONE',  ( 1.000000000000000000, 0.000000000000000000, 0.000000000000000000 ) ) ;
#8238 = ORIENTED_EDGE ( 'NONE', *, *, #3570, .F. ) ;
#8239 = VERTEX_POINT ( 'NONE', #3299 ) ;
#8240 = ADVANCED_FACE ( 'NONE', ( #8050 ), #2655, .F. ) ;
#8241 = AXIS2_PLACEMENT_3D ( 'NONE', #5010, #7628, #403 ) ;
#8242 = AXIS2_PLACEMENT_3D ( 'NONE', #1632, #3655, #342 ) ;
#8243 = CARTESIAN_POINT ( 'NONE',  ( -8.000000000000667910, -0.7805016046286897824, -8.399999999999657518 ) ) ;
#8244 = CARTESIAN_POINT ( 'NONE',  ( 7.999999999999563016, -4.618802153517398423, -7.685468820183672278 ) ) ;
#8245 = ORIENTED_EDGE ( 'NONE', *, *, #7365, .T. ) ;
#8246 = VECTOR ( 'NONE', #3113, 1000.000000000000114 ) ;
#8247 = DIRECTION ( 'NONE',  ( 0.000000000000000000, 0.000000000000000000, -1.000000000000000000 ) ) ;
#8248 = EDGE_CURVE ( 'NONE', #5078, #5384, #4386, .T. ) ;
#8249 = DIRECTION ( 'NONE',  ( -1.000000000000000000, 0.000000000000000000, 0.000000000000000000 ) ) ;
#8250 = EDGE_LOOP ( 'NONE', ( #1871, #8589, #4694 ) ) ;
#8251 = FACE_OUTER_BOUND ( 'NONE', #2837, .T. ) ;
#8252 = AXIS2_PLACEMENT_3D ( 'NONE', #628, #4115, #1458 ) ;
#8253 = ORIENTED_EDGE ( 'NONE', *, *, #3793, .T. ) ;
#8254 = FACE_OUTER_BOUND ( 'NONE', #3790, .T. ) ;
#8255 = DIRECTION ( 'NONE',  ( -1.000000000000000000, 1.774937036747276562E-30, 0.000000000000000000 ) ) ;
#8256 = DIRECTION ( 'NONE',  ( -7.703719777548943412E-34, 0.000000000000000000, 1.000000000000000000 ) ) ;
#8257 = ORIENTED_EDGE ( 'NONE', *, *, #1592, .F. ) ;
#8258 = AXIS2_PLACEMENT_3D ( 'NONE', #3812, #6468, #6360 ) ;
#8259 = DIRECTION ( 'NONE',  ( 8.659560562354952580E-17, 0.7071067811865491270, 0.7071067811865459074 ) ) ;
#8260 = EDGE_CURVE ( 'NONE', #838, #5265, #6671, .T. ) ;
#8261 = ORIENTED_EDGE ( 'NONE', *, *, #5043, .F. ) ;
#8262 = VECTOR ( 'NONE', #751, 1000.000000000000000 ) ;
#8263 = AXIS2_PLACEMENT_3D ( 'NONE', #1334, #7340, #3988 ) ;
#8264 = FACE_OUTER_BOUND ( 'NONE', #7311, .T. ) ;
#8265 = ORIENTED_EDGE ( 'NONE', *, *, #391, .F. ) ;
#8266 = B_SPLINE_CURVE_WITH_KNOTS ( 'NONE', 3,
 ( #951, #5534, #5632, #6839, #868, #3521, #6196, #2904 ),
 .UNSPECIFIED., .F., .F.,
 ( 4, 2, 2, 4 ),
 ( 0.004673709593151780146, 0.005837709341827351968, 0.007001709090502924657, 0.009329708587854070034 ),
 .UNSPECIFIED. ) ;
#8267 = CARTESIAN_POINT ( 'NONE',  ( 5.000000000000004441, -2.342598717236951789, 4.057500000000047180 ) ) ;
#8268 = EDGE_CURVE ( 'NONE', #2641, #5555, #7350, .T. ) ;
#8269 = CARTESIAN_POINT ( 'NONE',  ( 8.000000000000126121, -3.867591403079282397, -7.902324684675341437 ) ) ;
#8270 = EDGE_CURVE ( 'NONE', #3693, #5104, #6336, .T. ) ;
#8271 = FACE_OUTER_BOUND ( 'NONE', #4645, .T. ) ;
#8272 = PLANE ( 'NONE',  #3944 ) ;
#8273 = EDGE_LOOP ( 'NONE', ( #5742, #5766, #3491, #4662 ) ) ;
#8274 = EDGE_CURVE ( 'NONE', #7559, #838, #2299, .T. ) ;
#8275 = CARTESIAN_POINT ( 'NONE',  ( 0.000000000000000000, 0.000000000000000000, 0.000000000000000000 ) ) ;
#8276 = ORIENTED_EDGE ( 'NONE', *, *, #4048, .T. ) ;
#8277 = B_SPLINE_CURVE_WITH_KNOTS ( 'NONE', 3,
 ( #8325, #4076, #1691, #3634, #8243, #4365 ),
 .UNSPECIFIED., .F., .F.,
 ( 4, 2, 4 ),
 ( 0.008240550023493664611, 0.01057684187039431740, 0.01291313371729497193 ),
 .UNSPECIFIED. ) ;
#8278 = CONTEXT_DEPENDENT_SHAPE_REPRESENTATION ( #3115, #5740 ) ;
#8279 = EDGE_CURVE ( 'NONE', #4655, #982, #2744, .T. ) ;
#8280 = FACE_BOUND ( 'NONE', #3444, .T. ) ;
#8281 = CARTESIAN_POINT ( 'NONE',  ( -44.99999999999992895, 425.0000000000000000, 3.122502256758253953E-15 ) ) ;
#8282 = ORIENTED_EDGE ( 'NONE', *, *, #452, .F. ) ;
#8283 = EDGE_LOOP ( 'NONE', ( #6240, #2754, #1209, #971, #5801 ) ) ;
#8284 = SURFACE_STYLE_FILL_AREA ( #1570 ) ;
#8285 = PRODUCT_DEFINITION ( 'UNKNOWN', '', #4379, #7857 ) ;
#8286 = CARTESIAN_POINT ( 'NONE',  ( -4.000000000000003553, 6.928203230275431501, -8.400000000000018119 ) ) ;
#8287 = DIRECTION ( 'NONE',  ( 1.000000000000000000, 0.000000000000000000, 0.000000000000000000 ) ) ;
#8288 = VERTEX_POINT ( 'NONE', #6110 ) ;
#8289 = CARTESIAN_POINT ( 'NONE',  ( 0.000000000000000000, 0.000000000000000000, 0.000000000000000000 ) ) ;
#8290 = DIRECTION ( 'NONE',  ( 0.000000000000000000, 0.000000000000000000, 1.000000000000000000 ) ) ;
#8291 = CARTESIAN_POINT ( 'NONE',  ( -455.0000000000004547, 29.99999999999854694, 32.00000000000000000 ) ) ;
#8292 = VERTEX_POINT ( 'NONE', #7659 ) ;
#8293 = DIRECTION ( 'NONE',  ( 0.000000000000000000, 0.000000000000000000, -1.000000000000000000 ) ) ;
#8294 = ORIENTED_EDGE ( 'NONE', *, *, #5235, .T. ) ;
#8295 = FACE_OUTER_BOUND ( 'NONE', #3674, .T. ) ;
#8296 = ADVANCED_FACE ( 'NONE', ( #6928 ), #5868, .T. ) ;
#8297 = LINE ( 'NONE', #566, #6184 ) ;
#8298 = DIRECTION ( 'NONE',  ( 0.000000000000000000, 1.000000000000000000, 1.795949010423047374E-16 ) ) ;
#8299 = EDGE_LOOP ( 'NONE', ( #6224, #7268 ) ) ;
#8300 = DIRECTION ( 'NONE',  ( -1.463706757734299248E-32, 1.000000000000000000, 5.238529448733281520E-32 ) ) ;
#8301 = VECTOR ( 'NONE', #1340, 1000.000000000000000 ) ;
#8302 =( NAMED_UNIT ( * ) PLANE_ANGLE_UNIT ( ) SI_UNIT ( $, .RADIAN. ) );
#8303 = ORIENTED_EDGE ( 'NONE', *, *, #4501, .T. ) ;
#8304 = EDGE_LOOP ( 'NONE', ( #6857, #1820, #7603 ) ) ;
#8305 = DIRECTION ( 'NONE',  ( 0.000000000000000000, 5.322451846059955323E-30, -1.000000000000000000 ) ) ;
#8306 = AXIS2_PLACEMENT_3D ( 'NONE', #8039, #4028, #6011 ) ;
#8307 = EDGE_CURVE ( 'NONE', #4536, #5689, #2949, .T. ) ;
#8308 = FACE_OUTER_BOUND ( 'NONE', #5272, .T. ) ;
#8309 = DIRECTION ( 'NONE',  ( -1.000000000000000000, 3.549874073494553124E-30, 0.000000000000000000 ) ) ;
#8310 = DIRECTION ( 'NONE',  ( 1.000000000000000000, 0.000000000000000000, 0.000000000000000000 ) ) ;
#8311 = FACE_OUTER_BOUND ( 'NONE', #128, .T. ) ;
#8312 = CARTESIAN_POINT ( 'NONE',  ( 8.400000000000018119, -5.551115123125782702E-14, 6.661338147750939243E-13 ) ) ;
#8313 = ORIENTED_EDGE ( 'NONE', *, *, #576, .T. ) ;
#8314 = AXIS2_PLACEMENT_3D ( 'NONE', #658, #3135, #6486 ) ;
#8315 = DIRECTION ( 'NONE',  ( 0.000000000000000000, -1.064348848528640685E-29, 1.000000000000000000 ) ) ;
#8316 = VERTEX_POINT ( 'NONE', #206 ) ;
#8317 = ADVANCED_FACE ( 'NONE', ( #3522, #5679 ), #2256, .F. ) ;
#8318 = DIRECTION ( 'NONE',  ( 3.851859888774471706E-33, -7.598173571352216173E-18, 1.000000000000000000 ) ) ;
#8319 = DIRECTION ( 'NONE',  ( -1.000000000000000000, -8.881784197001244435E-16, 0.000000000000000000 ) ) ;
#8320 = ORIENTED_EDGE ( 'NONE', *, *, #8354, .T. ) ;
#8321 = DIRECTION ( 'NONE',  ( 0.9237280213470678847, 0.3830490080632384942, 0.000000000000000000 ) ) ;
#8322 = ADVANCED_FACE ( 'NONE', ( #2906 ), #7609, .F. ) ;
#8323 = EDGE_CURVE ( 'NONE', #1855, #8292, #960, .T. ) ;
#8324 = AXIS2_PLACEMENT_3D ( 'NONE', #4169, #344, #5677 ) ;
#8325 = CARTESIAN_POINT ( 'NONE',  ( -8.000000000000229150, -4.618802153516843312, -7.685468820183672278 ) ) ;
#8326 = ORIENTED_EDGE ( 'NONE', *, *, #6937, .T. ) ;
#8327 = DIRECTION ( 'NONE',  ( -1.000000000000000000, 1.774937036747276562E-30, -0.000000000000000000 ) ) ;
#8328 = DIRECTION ( 'NONE',  ( -6.938893903907228378E-17, 0.000000000000000000, -1.000000000000000000 ) ) ;
#8329 = APPLICATION_PROTOCOL_DEFINITION ( 'draft international standard', 'automotive_design', 1998, #6868 ) ;
#8330 = ORIENTED_EDGE ( 'NONE', *, *, #5620, .T. ) ;
#8331 = AXIS2_PLACEMENT_3D ( 'NONE', #371, #5020, #1750 ) ;
#8332 = EDGE_CURVE ( 'NONE', #2938, #4183, #2060, .T. ) ;
#8333 = DIRECTION ( 'NONE',  ( 0.000000000000000000, 0.000000000000000000, 1.000000000000000000 ) ) ;
#8334 = DIRECTION ( 'NONE',  ( 0.7071067811865474617, 8.659560562354431192E-17, 0.7071067811865474617 ) ) ;
#8335 = VECTOR ( 'NONE', #1166, 1000.000000000000000 ) ;
#8336 = VERTEX_POINT ( 'NONE', #8179 ) ;
#8337 = FACE_OUTER_BOUND ( 'NONE', #1089, .T. ) ;
#8338 = ORIENTED_EDGE ( 'NONE', *, *, #6251, .F. ) ;
#8339 = EDGE_CURVE ( 'NONE', #4775, #6636, #7531, .T. ) ;
#8340 = VERTEX_POINT ( 'NONE', #4261 ) ;
#8341 = AXIS2_PLACEMENT_3D ( 'NONE', #1533, #4189, #6860 ) ;
#8342 = DIRECTION ( 'NONE',  ( 1.000000000000000000, 0.000000000000000000, 0.000000000000000000 ) ) ;
#8343 = PRODUCT ( 'hex nut style 1_am_B18.2.4.1M - Hex nut, Style 1,  M10 x 1.5, with 16mm WAF --D-N', 'hex nut style 1_am_B18.2.4.1M - Hex nut, Style 1,  M10 x 1.5, with 16mm WAF --D-N', '', ( #8375 ) ) ;
#8344 = ORIENTED_EDGE ( 'NONE', *, *, #3734, .T. ) ;
#8345 = DIRECTION ( 'NONE',  ( 1.000000000000000000, 8.881784197001244435E-16, 0.000000000000000000 ) ) ;
#8346 = AXIS2_PLACEMENT_3D ( 'NONE', #2770, #8042, #1374 ) ;
#8347 = AXIS2_PLACEMENT_3D ( 'NONE', #5658, #1536, #4848 ) ;
#8348 = AXIS2_PLACEMENT_3D ( 'NONE', #8500, #7243, #5240 ) ;
#8349 = CARTESIAN_POINT ( 'NONE',  ( 0.000000000000000000, 0.000000000000000000, 10.00000000000000888 ) ) ;
#8350 = CARTESIAN_POINT ( 'NONE',  ( -8.000000000000671463, 3.115336682267233481, -8.080606868608098736 ) ) ;
#8351 = FILL_AREA_STYLE ('',( #5157 ) ) ;
#8352 = DIRECTION ( 'NONE',  ( -1.000000000000000000, 2.842664852890546338E-35, -7.703719777548943412E-34 ) ) ;
#8353 = DIRECTION ( 'NONE',  ( 0.9237280213470678847, 0.3830490080632384942, 0.000000000000000000 ) ) ;
#8354 = EDGE_CURVE ( 'NONE', #6000, #2499, #5400, .T. ) ;
#8355 = PLANE ( 'NONE',  #6589 ) ;
#8356 = ORIENTED_EDGE ( 'NONE', *, *, #4471, .F. ) ;
#8357 = EDGE_CURVE ( 'NONE', #18, #4707, #3392, .T. ) ;
#8358 = PRODUCT_DEFINITION_SHAPE ( 'NONE', 'NONE',  #8621 ) ;
#8359 = CARTESIAN_POINT ( 'NONE',  ( 2.220446049250313081E-13, -9.237604307034242623, -8.400000000000018119 ) ) ;
#8360 = ORIENTED_EDGE ( 'NONE', *, *, #5738, .F. ) ;
#8361 = PRESENTATION_LAYER_ASSIGNMENT (  '', '', ( #5446 ) ) ;
#8362 = CARTESIAN_POINT ( 'NONE',  ( -50.00000000000004263, 425.0000000000000000, 3.469446951953614189E-15 ) ) ;
#8363 = CONTEXT_DEPENDENT_SHAPE_REPRESENTATION ( #3531, #4745 ) ;
#8364 = DIRECTION ( 'NONE',  ( 1.000000000000000000, 3.083952846180997183E-15, -4.108650548026112028E-30 ) ) ;
#8365 = EDGE_LOOP ( 'NONE', ( #655, #7522, #1274 ) ) ;
#8366 = DIRECTION ( 'NONE',  ( -1.000000000000000000, 1.774937036747276562E-30, 0.000000000000000000 ) ) ;
#8367 = EDGE_CURVE ( 'NONE', #1742, #6630, #750, .T. ) ;
#8368 = UNCERTAINTY_MEASURE_WITH_UNIT (LENGTH_MEASURE( 1.000000000000000082E-05 ), #4544, 'distance_accuracy_value', 'NONE');
#8369 = DIRECTION ( 'NONE',  ( 0.000000000000000000, -1.024214141749972931E-29, 1.000000000000000000 ) ) ;
#8370 = EDGE_CURVE ( 'NONE', #4915, #7471, #2410, .T. ) ;
#8371 = CARTESIAN_POINT ( 'NONE',  ( 2.254359249602142680E-58, 6.350533013084927146E-29, -5.700000000000001954 ) ) ;
#8372 = CARTESIAN_POINT ( 'NONE',  ( 4.000000000000003553, 9.714451465470119729E-14, 0.000000000000000000 ) ) ;
#8373 = ORIENTED_EDGE ( 'NONE', *, *, #8022, .F. ) ;
#8374 = FACE_OUTER_BOUND ( 'NONE', #7971, .T. ) ;
#8375 = PRODUCT_CONTEXT ( 'NONE', #5988, 'mechanical' ) ;
#8376 = CONICAL_SURFACE ( 'NONE', #126, 8.000000000000007105, 1.047197551196597631 ) ;
#8377 = AXIS2_PLACEMENT_3D ( 'NONE', #6136, #4773, #143 ) ;
#8378 = ADVANCED_FACE ( 'NONE', ( #2335 ), #5724, .F. ) ;
#8379 = CARTESIAN_POINT ( 'NONE',  ( -49.99999999999963762, 87.50000000000035527, 9.999999999999786837 ) ) ;
#8380 = ORIENTED_EDGE ( 'NONE', *, *, #7240, .T. ) ;
#8381 = FACE_OUTER_BOUND ( 'NONE', #7331, .T. ) ;
#8382 = CIRCLE ( 'NONE', #4631, 4.250000000000010658 ) ;
#8383 =( NAMED_UNIT ( * ) PLANE_ANGLE_UNIT ( ) SI_UNIT ( $, .RADIAN. ) );
#8384 = ORIENTED_EDGE ( 'NONE', *, *, #5812, .T. ) ;
#8385 = CARTESIAN_POINT ( 'NONE',  ( -2.220446049250313081E-13, -650.0000000000000000, 79.99999999999995737 ) ) ;
#8386 = VERTEX_POINT ( 'NONE', #4828 ) ;
#8387 = DIRECTION ( 'NONE',  ( 0.000000000000000000, 1.953992523340276458E-14, -1.000000000000000000 ) ) ;
#8388 = FACE_BOUND ( 'NONE', #7021, .T. ) ;
#8389 = CIRCLE ( 'NONE', #7830, 24.50000000000001066 ) ;
#8390 = ADVANCED_FACE ( 'NONE', ( #4217 ), #3675, .T. ) ;
#8391 = DIRECTION ( 'NONE',  ( -0.5000000000000042188, -3.721909990733644056E-30, 0.8660254037844361541 ) ) ;
#8392 = ADVANCED_FACE ( 'NONE', ( #3571, #6236 ), #8272, .F. ) ;
#8393 = CARTESIAN_POINT ( 'NONE',  ( 7.999999999999340972, -4.618802153516732290, -0.7145311798163467287 ) ) ;
#8394 = DIRECTION ( 'NONE',  ( -1.000000000000000000, -8.881784197001244435E-16, 0.000000000000000000 ) ) ;
#8395 = CARTESIAN_POINT ( 'NONE',  ( -50.00000000000004263, -425.0000000000000000, 3.469446951953614189E-15 ) ) ;
#8396 = AXIS2_PLACEMENT_3D ( 'NONE', #179, #6168, #5547 ) ;
#8397 = CARTESIAN_POINT ( 'NONE',  ( -3.660532965668688909, 7.124194613927615549, -8.400000000000062528 ) ) ;
#8398 = ORIENTED_EDGE ( 'NONE', *, *, #5342, .T. ) ;
#8399 = CARTESIAN_POINT ( 'NONE',  ( 8.400000000000018119, 9.010270651821244215E-27, 4.000000000000696332 ) ) ;
#8400 = ORIENTED_EDGE ( 'NONE', *, *, #3956, .F. ) ;
#8401 = AXIS2_PLACEMENT_3D ( 'NONE', #3553, #6095, #4071 ) ;
#8402 = AXIS2_PLACEMENT_3D ( 'NONE', #5335, #2019, #6639 ) ;
#8403 = CARTESIAN_POINT ( 'NONE',  ( 8.000000000000229150, 4.618802153516954334, -8.400000000000018119 ) ) ;
#8404 = EDGE_CURVE ( 'NONE', #2630, #2559, #1003, .T. ) ;
#8405 = B_SPLINE_CURVE_WITH_KNOTS ( 'NONE', 3,
 ( #5315, #2003, #2571, #5226, #1350, #7354 ),
 .UNSPECIFIED., .F., .F.,
 ( 4, 2, 4 ),
 ( 2.380731631918174131E-07, 0.002336973833157790156, 0.004673709593152389034 ),
 .UNSPECIFIED. ) ;
#8406 = DIRECTION ( 'NONE',  ( 1.000000000000000000, -0.000000000000000000, -6.938893903907228378E-17 ) ) ;
#8407 = ORIENTED_EDGE ( 'NONE', *, *, #3461, .T. ) ;
#8408 = EDGE_LOOP ( 'NONE', ( #6682, #4686, #1537, #3703 ) ) ;
#8409 = DIRECTION ( 'NONE',  ( -3.851859888774471706E-33, 7.598173571352223877E-18, -1.000000000000000000 ) ) ;
#8410 = CARTESIAN_POINT ( 'NONE',  ( -4.000000000000114575, -6.928203230275487456, 0.000000000000000000 ) ) ;
#8411 = EDGE_CURVE ( 'NONE', #4726, #4794, #5489, .T. ) ;
#8412 = FACE_OUTER_BOUND ( 'NONE', #5186, .T. ) ;
#8413 = CARTESIAN_POINT ( 'NONE',  ( 8.000000000000234479, -0.7805016046292178045, -8.399999999999876010 ) ) ;
#8414 = ADVANCED_FACE ( 'NONE', ( #7213 ), #2463, .T. ) ;
#8415 = VECTOR ( 'NONE', #6460, 1000.000000000000000 ) ;
#8416 = LINE ( 'NONE', #2440, #3375 ) ;
#8417 = CARTESIAN_POINT ( 'NONE',  ( -4.000000000000003553, -6.928203230275431501, 0.000000000000000000 ) ) ;
#8418 = VERTEX_POINT ( 'NONE', #3078 ) ;
#8419 = LINE ( 'NONE', #6585, #3372 ) ;
#8420 = CARTESIAN_POINT ( 'NONE',  ( 9.184850993605153466E-15, 295.0000000000000568, -75.00000000000009948 ) ) ;
#8421 = AXIS2_PLACEMENT_3D ( 'NONE', #4527, #8409, #2436 ) ;
#8422 = DIRECTION ( 'NONE',  ( -0.000000000000000000, -0.000000000000000000, 1.000000000000000000 ) ) ;
#8423 = SHAPE_DEFINITION_REPRESENTATION ( #8483, #6969 ) ;
#8424 = ADVANCED_FACE ( 'NONE', ( #7863 ), #1768, .T. ) ;
#8425 = ORIENTED_EDGE ( 'NONE', *, *, #866, .F. ) ;
#8426 = DIRECTION ( 'NONE',  ( -1.000000000000000000, 0.000000000000000000, 0.000000000000000000 ) ) ;
#8427 = VECTOR ( 'NONE', #6702, 1000.000000000000000 ) ;
#8428 = ORIENTED_EDGE ( 'NONE', *, *, #4418, .F. ) ;
#8429 = CARTESIAN_POINT ( 'NONE',  ( -1.310872448937805634, 8.480771745766437775, -0.3173508448886594446 ) ) ;
#8430 = ORIENTED_EDGE ( 'NONE', *, *, #1747, .T. ) ;
#8431 = DIRECTION ( 'NONE',  ( -1.000000000000000000, -8.881784197001244435E-16, 0.000000000000000000 ) ) ;
#8432 = AXIS2_PLACEMENT_3D ( 'NONE', #5155, #1040, #2507 ) ;
#8433 = DIRECTION ( 'NONE',  ( 3.919652622816902408E-30, 3.944304526105059027E-30, -1.000000000000000000 ) ) ;
#8434 = DIRECTION ( 'NONE',  ( -7.703719777548943412E-34, 0.000000000000000000, 1.000000000000000000 ) ) ;
#8435 = DIRECTION ( 'NONE',  ( 1.000000000000000000, 0.000000000000000000, 0.000000000000000000 ) ) ;
#8436 = DIRECTION ( 'NONE',  ( 0.000000000000000000, 0.000000000000000000, -1.000000000000000000 ) ) ;
#8437 = CARTESIAN_POINT ( 'NONE',  ( 0.000000000000000000, -9.237604307034075646, -0.7145311798163467287 ) ) ;
#8438 = CARTESIAN_POINT ( 'NONE',  ( -99.99999999999972999, 0.000000000000000000, 9.999999999999980460 ) ) ;
#8439 = ORIENTED_EDGE ( 'NONE', *, *, #7145, .T. ) ;
#8440 = ORIENTED_EDGE ( 'NONE', *, *, #1046, .F. ) ;
#8441 = CARTESIAN_POINT ( 'NONE',  ( 8.000000000000008882, 3.115336682267075830, -8.080606868608489535 ) ) ;
#8442 = CONTEXT_DEPENDENT_SHAPE_REPRESENTATION ( #2067, #5434 ) ;
#8443 = DIRECTION ( 'NONE',  ( -3.919652622816902408E-30, -3.944304526105059027E-30, 1.000000000000000000 ) ) ;
#8444 = ORIENTED_EDGE ( 'NONE', *, *, #4196, .T. ) ;
#8445 = ORIENTED_EDGE ( 'NONE', *, *, #2618, .T. ) ;
#8446 = DIRECTION ( 'NONE',  ( -1.000000000000000000, -8.881784197001244435E-16, 0.000000000000000000 ) ) ;
#8447 = ADVANCED_FACE ( 'NONE', ( #3123 ), #5808, .F. ) ;
#8448 = DIRECTION ( 'NONE',  ( -1.034996974062495478E-32, 0.7071067811865459074, 0.7071067811865491270 ) ) ;
#8449 = CARTESIAN_POINT ( 'NONE',  ( 0.000000000000000000, 9.237604307034130713, -0.7145311798163467287 ) ) ;
#8450 = CARTESIAN_POINT ( 'NONE',  ( -8.000000000000229150, 4.618802153516954334, -8.400000000000018119 ) ) ;
#8451 = ORIENTED_EDGE ( 'NONE', *, *, #5252, .T. ) ;
#8452 = CARTESIAN_POINT ( 'NONE',  ( -3.318518101603002535, -7.321656987763293323, -8.399999999999796074 ) ) ;
#8453 = CARTESIAN_POINT ( 'NONE',  ( 3.660532965668853667, -7.124194613927719466, -8.399999999999964828 ) ) ;
#8454 = LINE ( 'NONE', #1745, #7923 ) ;
#8455 = DIRECTION ( 'NONE',  ( -1.058471975245261993E-16, 8.736544766236848795E-16, -1.000000000000000000 ) ) ;
#8456 = EDGE_CURVE ( 'NONE', #6623, #173, #7697, .T. ) ;
#8457 = CARTESIAN_POINT ( 'NONE',  ( 44.99999999999992895, 425.0000000000000000, -3.122502256758253953E-15 ) ) ;
#8458 = ORIENTED_EDGE ( 'NONE', *, *, #6479, .T. ) ;
#8459 = AXIS2_PLACEMENT_3D ( 'NONE', #4977, #7036, #3724 ) ;
#8460 = DIRECTION ( 'NONE',  ( 0.000000000000000000, 0.000000000000000000, 1.000000000000000000 ) ) ;
#8461 = VERTEX_POINT ( 'NONE', #1724 ) ;
#8462 = EDGE_CURVE ( 'NONE', #5093, #6484, #5345, .T. ) ;
#8463 = CARTESIAN_POINT ( 'NONE',  ( 5.080504117408889186, 2.106769544347817824, 0.000000000000000000 ) ) ;
#8464 = ORIENTED_EDGE ( 'NONE', *, *, #6092, .F. ) ;
#8465 = CARTESIAN_POINT ( 'NONE',  ( 44.99999999999992895, 425.0000000000000000, -25.00000000000001066 ) ) ;
#8466 = CARTESIAN_POINT ( 'NONE',  ( 33.00000000000055422, -1.386389088789023606E-14, -3.309499999993116504 ) ) ;
#8467 = DIRECTION ( 'NONE',  ( 0.000000000000000000, 0.000000000000000000, -1.000000000000000000 ) ) ;
#8468 = CIRCLE ( 'NONE', #5127, 8.000000000000007105 ) ;
#8469 = DIRECTION ( 'NONE',  ( -7.703719777548943412E-34, 0.000000000000000000, 1.000000000000000000 ) ) ;
#8470 = EDGE_CURVE ( 'NONE', #3749, #902, #2530, .T. ) ;
#8471 = DIRECTION ( 'NONE',  ( -3.851859888774471706E-33, 7.598173571352223877E-18, -1.000000000000000000 ) ) ;
#8472 = FACE_BOUND ( 'NONE', #7187, .T. ) ;
#8473 = CARTESIAN_POINT ( 'NONE',  ( 0.000000000000000000, 60.00000000000000000, 50.00000000000000000 ) ) ;
#8474 = ORIENTED_EDGE ( 'NONE', *, *, #3146, .T. ) ;
#8475 = VECTOR ( 'NONE', #5966, 999.9999999999998863 ) ;
#8476 = ORIENTED_EDGE ( 'NONE', *, *, #2250, .T. ) ;
#8477 = DIRECTION ( 'NONE',  ( 1.000000000000000000, -0.000000000000000000, -6.938893903907228378E-17 ) ) ;
#8478 = AXIS2_PLACEMENT_3D ( 'NONE', #4192, #3551, #6220 ) ;
#8479 = CIRCLE ( 'NONE', #4237, 5.500000000000000000 ) ;
#8480 = FACE_BOUND ( 'NONE', #8523, .T. ) ;
#8481 = CIRCLE ( 'NONE', #2110, 4.499999999999993783 ) ;
#8482 = AXIS2_PLACEMENT_3D ( 'NONE', #7575, #3659, #8315 ) ;
#8483 = PRODUCT_DEFINITION_SHAPE ( 'NONE', 'NONE',  #7017 ) ;
#8484 = CARTESIAN_POINT ( 'NONE',  ( 0.000000000000000000, 0.000000000000000000, 0.000000000000000000 ) ) ;
#8485 = AXIS2_PLACEMENT_3D ( 'NONE', #4929, #7109, #8287 ) ;
#8486 = ORIENTED_EDGE ( 'NONE', *, *, #6627, .F. ) ;
#8487 =( GEOMETRIC_REPRESENTATION_CONTEXT ( 3 ) GLOBAL_UNCERTAINTY_ASSIGNED_CONTEXT ( ( #6834 ) ) GLOBAL_UNIT_ASSIGNED_CONTEXT ( ( #4823, #819, #4163 ) ) REPRESENTATION_CONTEXT ( 'NONE', 'WORKASPACE' ) );
#8488 = DIRECTION ( 'NONE',  ( -7.703719777548943412E-34, 0.000000000000000000, 1.000000000000000000 ) ) ;
#8489 = VERTEX_POINT ( 'NONE', #593 ) ;
#8490 = ORIENTED_EDGE ( 'NONE', *, *, #5969, .F. ) ;
#8491 = ORIENTED_EDGE ( 'NONE', *, *, #5062, .F. ) ;
#8492 = CARTESIAN_POINT ( 'NONE',  ( -5.080504117408890075, -2.106769544347818712, -8.400000000000018119 ) ) ;
#8493 = CARTESIAN_POINT ( 'NONE',  ( 44.99999999999992895, 500.0000000000000000, -45.00000000000000711 ) ) ;
#8494 = ADVANCED_FACE ( 'NONE', ( #3900 ), #8355, .F. ) ;
#8495 = EDGE_LOOP ( 'NONE', ( #2134, #6170, #2414, #4287, #6865, #2014 ) ) ;
#8496 = PLANE ( 'NONE',  #6573 ) ;
#8497 = APPLICATION_PROTOCOL_DEFINITION ( 'draft international standard', 'automotive_design', 1998, #5661 ) ;
#8498 = EDGE_CURVE ( 'NONE', #4183, #2938, #5639, .T. ) ;
#8499 = EDGE_LOOP ( 'NONE', ( #1483, #4199, #8053, #4070 ) ) ;
#8500 = CARTESIAN_POINT ( 'NONE',  ( 8.000000000000007105, 2.775557561562891351E-14, 6.661338147750939243E-13 ) ) ;
#8501 = DIRECTION ( 'NONE',  ( -1.000000000000000000, -8.881784197001244435E-16, 0.000000000000000000 ) ) ;
#8502 = ORIENTED_EDGE ( 'NONE', *, *, #6092, .T. ) ;
#8503 = VECTOR ( 'NONE', #721, 1000.000000000000000 ) ;
#8504 = CARTESIAN_POINT ( 'NONE',  ( 0.6543471694407195782, 8.859816792613939285, -0.4964154566689378267 ) ) ;
#8505 = VERTEX_POINT ( 'NONE', #6556 ) ;
#8506 = DIRECTION ( 'NONE',  ( 0.000000000000000000, 5.322451846059955323E-30, -1.000000000000000000 ) ) ;
#8507 = EDGE_CURVE ( 'NONE', #5902, #1856, #6296, .T. ) ;
#8508 = DIRECTION ( 'NONE',  ( 0.000000000000000000, 0.000000000000000000, 1.000000000000000000 ) ) ;
#8509 = CIRCLE ( 'NONE', #4078, 3.047499999999999876 ) ;
#8510 = CARTESIAN_POINT ( 'NONE',  ( 0.6543471694413475204, 8.859816792613639080, -0.4964154566687958292 ) ) ;
#8511 = DIRECTION ( 'NONE',  ( 0.000000000000000000, -0.000000000000000000, 1.000000000000000000 ) ) ;
#8512 = CARTESIAN_POINT ( 'NONE',  ( 0.000000000000000000, 0.000000000000000000, 18.00000000000000355 ) ) ;
#8513 = VERTEX_POINT ( 'NONE', #6475 ) ;
#8514 =( NAMED_UNIT ( * ) PLANE_ANGLE_UNIT ( ) SI_UNIT ( $, .RADIAN. ) );
#8515 = ORIENTED_EDGE ( 'NONE', *, *, #7492, .T. ) ;
#8516 = FACE_OUTER_BOUND ( 'NONE', #1826, .T. ) ;
#8517 = CONICAL_SURFACE ( 'NONE', #1983, 8.000000000000007105, 1.047197551196597631 ) ;
#8518 = CIRCLE ( 'NONE', #4778, 5.500000000000023981 ) ;
#8519 = ADVANCED_FACE ( 'NONE', ( #6512, #511 ), #5846, .T. ) ;
#8520 = CARTESIAN_POINT ( 'NONE',  ( 8.000000000000232703, 0.7809653281575149597, -1.284508523852201883E-13 ) ) ;
#8521 = DIRECTION ( 'NONE',  ( 0.000000000000000000, 1.000000000000000000, 0.000000000000000000 ) ) ;
#8522 = CONTEXT_DEPENDENT_SHAPE_REPRESENTATION ( #4174, #8081 ) ;
#8523 = EDGE_LOOP ( 'NONE', ( #6685, #8380 ) ) ;
#8524 = CARTESIAN_POINT ( 'NONE',  ( 2.645508037661676859, 7.710219529346706402, -8.331901280394584219 ) ) ;
#8525 = CIRCLE ( 'NONE', #336, 5.749999999999985789 ) ;
#8526 = ORIENTED_EDGE ( 'NONE', *, *, #2678, .T. ) ;
#8527 = ORIENTED_EDGE ( 'NONE', *, *, #1594, .F. ) ;
#8528 = CIRCLE ( 'NONE', #4087, 5.499999999999999112 ) ;
#8529 = AXIS2_PLACEMENT_3D ( 'NONE', #5036, #4468, #6401 ) ;
#8530 = PLANE ( 'NONE',  #5617 ) ;
#8531 = EDGE_LOOP ( 'NONE', ( #3258, #560 ) ) ;
#8532 = DIRECTION ( 'NONE',  ( 1.000000000000000000, 8.881784197001244435E-16, 0.000000000000000000 ) ) ;
#8533 = CARTESIAN_POINT ( 'NONE',  ( -5.690023276062584401, -5.952467836904117959, -8.269346954796148452 ) ) ;
#8534 = CARTESIAN_POINT ( 'NONE',  ( 0.000000000000000000, -9.237604307034075646, -7.685468820183672278 ) ) ;
#8535 = SURFACE_STYLE_FILL_AREA ( #4486 ) ;
#8536 = EDGE_LOOP ( 'NONE', ( #790, #2886 ) ) ;
#8537 = LINE ( 'NONE', #6537, #880 ) ;
#8538 = EDGE_CURVE ( 'NONE', #1999, #6850, #4089, .T. ) ;
#8539 = EDGE_CURVE ( 'NONE', #7164, #6339, #6907, .T. ) ;
#8540 = ORIENTED_EDGE ( 'NONE', *, *, #5520, .T. ) ;
#8541 = PLANE ( 'NONE',  #7782 ) ;
#8542 = ORIENTED_EDGE ( 'NONE', *, *, #5373, .F. ) ;
#8543 = CARTESIAN_POINT ( 'NONE',  ( 4.000000000000003553, 6.928203230275431501, 0.000000000000000000 ) ) ;
#8544 = PRODUCT_DEFINITION_SHAPE ( 'NONE', 'NONE',  #297 ) ;
#8545 = ORIENTED_EDGE ( 'NONE', *, *, #4162, .T. ) ;
#8546 = CARTESIAN_POINT ( 'NONE',  ( -50.00000000000004263, 500.0000000000000000, 50.00000000000000000 ) ) ;
#8547 = ADVANCED_FACE ( 'NONE', ( #6651 ), #2690, .F. ) ;
#8548 = PRODUCT_DEFINITION_CONTEXT ( 'detailed design', #7088, 'design' ) ;
#8549 = FACE_OUTER_BOUND ( 'NONE', #2532, .T. ) ;
#8550 = DIRECTION ( 'NONE',  ( -0.5000000000000041078, 0.8660254037844363761, 0.000000000000000000 ) ) ;
#8551 = DIRECTION ( 'NONE',  ( -1.000000000000000000, 1.774937036747276562E-30, 0.000000000000000000 ) ) ;
#8552 = DIRECTION ( 'NONE',  ( -0.000000000000000000, -0.000000000000000000, 1.000000000000000000 ) ) ;
#8553 = DIRECTION ( 'NONE',  ( 1.000000000000000000, -0.000000000000000000, -6.938893903907228378E-17 ) ) ;
#8554 = SURFACE_STYLE_FILL_AREA ( #3251 ) ;
#8555 = ORIENTED_EDGE ( 'NONE', *, *, #3699, .T. ) ;
#8556 = B_SPLINE_CURVE_WITH_KNOTS ( 'NONE', 3,
 ( #388, #7128, #3163, #7049, #6400, #1767, #433, #3779 ),
 .UNSPECIFIED., .F., .F.,
 ( 4, 2, 2, 4 ),
 ( 0.004673709593152389034, 0.005837709341827845497, 0.007001709090503301092, 0.009329708587854212282 ),
 .UNSPECIFIED. ) ;
#8557 = FACE_OUTER_BOUND ( 'NONE', #2737, .T. ) ;
#8558 = EDGE_CURVE ( 'NONE', #8316, #5838, #1466, .T. ) ;
#8559 = UNCERTAINTY_MEASURE_WITH_UNIT (LENGTH_MEASURE( 1.000000000000000082E-05 ), #7989, 'distance_accuracy_value', 'NONE');
#8560 = AXIS2_PLACEMENT_3D ( 'NONE', #2173, #59, #6791 ) ;
#8561 = CARTESIAN_POINT ( 'NONE',  ( -8.000000000000225597, -0.7805016046291550769, -1.288946976495813912E-13 ) ) ;
#8562 = CARTESIAN_POINT ( 'NONE',  ( 8.000000000000232703, 1.572549600175502604, -0.06894455525524925688 ) ) ;
#8563 = CARTESIAN_POINT ( 'NONE',  ( -5.354491962338109090, 6.146186931204312920, -0.06809871960538033120 ) ) ;
#8564 = ORIENTED_EDGE ( 'NONE', *, *, #8192, .T. ) ;
#8565 = CARTESIAN_POINT ( 'NONE',  ( 8.000000000000007105, -4.618802153517121312, -0.7145311798163467287 ) ) ;
#8566 = EDGE_LOOP ( 'NONE', ( #2897, #2661, #2589, #3367 ) ) ;
#8567 = ORIENTED_EDGE ( 'NONE', *, *, #8219, .T. ) ;
#8568 = ADVANCED_FACE ( 'NONE', ( #5438 ), #4782, .F. ) ;
#8569 = CARTESIAN_POINT ( 'NONE',  ( -1.313474075707481648, -8.479269695850799593, -8.083279549040190304 ) ) ;
#8570 = ORIENTED_EDGE ( 'NONE', *, *, #3994, .T. ) ;
#8571 = CARTESIAN_POINT ( 'NONE',  ( -36.74999999999997158, 3.469446951953614189E-15, -6.938893903907228378E-15 ) ) ;
#8572 = EDGE_CURVE ( 'NONE', #8513, #6375, #1428, .T. ) ;
#8573 = FACE_OUTER_BOUND ( 'NONE', #1038, .T. ) ;
#8574 = DIRECTION ( 'NONE',  ( 0.000000000000000000, 1.064348848528640405E-29, -1.000000000000000000 ) ) ;
#8575 = AXIS2_PLACEMENT_3D ( 'NONE', #3448, #6116, #2833 ) ;
#8576 = DIRECTION ( 'NONE',  ( 0.000000000000000000, 0.000000000000000000, -1.000000000000000000 ) ) ;
#8577 = FACE_OUTER_BOUND ( 'NONE', #127, .T. ) ;
#8578 = EDGE_LOOP ( 'NONE', ( #6038, #1564, #4570, #4542 ) ) ;
#8579 = DIRECTION ( 'NONE',  ( 0.000000000000000000, 0.000000000000000000, 1.000000000000000000 ) ) ;
#8580 = ADVANCED_FACE ( 'NONE', ( #6102 ), #7387, .F. ) ;
#8581 = APPLICATION_CONTEXT ( 'automotive_design' ) ;
#8582 = APPLICATION_PROTOCOL_DEFINITION ( 'draft international standard', 'automotive_design', 1998, #3030 ) ;
#8583 = DIRECTION ( 'NONE',  ( -1.000000000000000000, -1.776356839400249676E-15, 0.000000000000000000 ) ) ;
#8584 = ORIENTED_EDGE ( 'NONE', *, *, #6341, .F. ) ;
#8585 = CARTESIAN_POINT ( 'NONE',  ( 8.000000000000229150, 3.871967595402076689, -7.901061386767455730 ) ) ;
#8586 = EDGE_CURVE ( 'NONE', #4804, #7189, #7906, .T. ) ;
#8587 = AXIS2_PLACEMENT_3D ( 'NONE', #8281, #6207, #1522 ) ;
#8588 = CARTESIAN_POINT ( 'NONE',  ( 3.020215680056619492E-16, -425.0000000000000568, -8.673617379884035472E-16 ) ) ;
#8589 = ORIENTED_EDGE ( 'NONE', *, *, #7620, .F. ) ;
#8590 = AXIS2_PLACEMENT_3D ( 'NONE', #1462, #4119, #2811 ) ;
#8591 = CARTESIAN_POINT ( 'NONE',  ( -7.999999999999998224, -1.555946510856077492, -0.06708870216334689163 ) ) ;
#8592 = EDGE_LOOP ( 'NONE', ( #3772, #3796, #502, #4092, #3650, #2680 ) ) ;
#8593 = CARTESIAN_POINT ( 'NONE',  ( -4.250000000000000888, 32.50000000000005684, -6.938893903907228378E-15 ) ) ;
#8594 = DIRECTION ( 'NONE',  ( -1.000000000000000000, 2.842664852890546338E-35, 1.540743955509788340E-33 ) ) ;
#8595 = DIRECTION ( 'NONE',  ( 3.851859888774471706E-33, -7.598173571352223877E-18, 1.000000000000000000 ) ) ;
#8596 = CARTESIAN_POINT ( 'NONE',  ( 0.000000000000000000, 1.759474945355512965, -3.047500000000091802 ) ) ;
#8597 = ADVANCED_FACE ( 'NONE', ( #7953 ), #7835, .T. ) ;
#8598 = FACE_BOUND ( 'NONE', #6912, .T. ) ;
#8599 = CARTESIAN_POINT ( 'NONE',  ( 10.40000000000001990, -4.129221776824974572E-28, 5.000000000000478728 ) ) ;
#8600 = ORIENTED_EDGE ( 'NONE', *, *, #87, .F. ) ;
#8601 = DIRECTION ( 'NONE',  ( 1.000000000000000000, -1.284024588418159817E-35, 0.000000000000000000 ) ) ;
#8602 = FILL_AREA_STYLE ('',( #102 ) ) ;
#8603 = DIRECTION ( 'NONE',  ( 1.463706757734299248E-32, -1.000000000000000000, -5.238529448733281520E-32 ) ) ;
#8604 = EDGE_CURVE ( 'NONE', #7000, #2630, #7703, .T. ) ;
#8605 = NEXT_ASSEMBLY_USAGE_OCCURRENCE ( 'NAUO1', ' ', ' ', #4551, #7892, $ ) ;
#8606 = NEXT_ASSEMBLY_USAGE_OCCURRENCE ( 'NAUO2', ' ', ' ', #4551, #8285, $ ) ;
#8607 = NEXT_ASSEMBLY_USAGE_OCCURRENCE ( 'NAUO3', ' ', ' ', #4551, #7892, $ ) ;
#8608 = NEXT_ASSEMBLY_USAGE_OCCURRENCE ( 'NAUO4', ' ', ' ', #4551, #8285, $ ) ;
#8609 = NEXT_ASSEMBLY_USAGE_OCCURRENCE ( 'NAUO5', ' ', ' ', #4551, #2753, $ ) ;
#8610 = NEXT_ASSEMBLY_USAGE_OCCURRENCE ( 'NAUO6', ' ', ' ', #4551, #4290, $ ) ;
#8611 = NEXT_ASSEMBLY_USAGE_OCCURRENCE ( 'NAUO7', ' ', ' ', #4551, #297, $ ) ;
#8612 = NEXT_ASSEMBLY_USAGE_OCCURRENCE ( 'NAUO8', ' ', ' ', #4551, #4926, $ ) ;
#8613 = NEXT_ASSEMBLY_USAGE_OCCURRENCE ( 'NAUO9', ' ', ' ', #4551, #4290, $ ) ;
#8614 = NEXT_ASSEMBLY_USAGE_OCCURRENCE ( 'NAUO10', ' ', ' ', #4551, #297, $ ) ;
#8615 = NEXT_ASSEMBLY_USAGE_OCCURRENCE ( 'NAUO11', ' ', ' ', #4551, #4926, $ ) ;
#8616 = NEXT_ASSEMBLY_USAGE_OCCURRENCE ( 'NAUO12', ' ', ' ', #4551, #5591, $ ) ;
#8617 = NEXT_ASSEMBLY_USAGE_OCCURRENCE ( 'NAUO13', ' ', ' ', #4551, #5591, $ ) ;
#8618 = NEXT_ASSEMBLY_USAGE_OCCURRENCE ( 'NAUO14', ' ', ' ', #4551, #5591, $ ) ;
#8619 = NEXT_ASSEMBLY_USAGE_OCCURRENCE ( 'NAUO15', ' ', ' ', #4551, #5591, $ ) ;
#8620 = NEXT_ASSEMBLY_USAGE_OCCURRENCE ( 'NAUO16', ' ', ' ', #4551, #944, $ ) ;
#8621 = NEXT_ASSEMBLY_USAGE_OCCURRENCE ( 'NAUO17', ' ', ' ', #4551, #944, $ ) ;
#8622 = NEXT_ASSEMBLY_USAGE_OCCURRENCE ( 'NAUO18', ' ', ' ', #4551, #944, $ ) ;
#8623 = NEXT_ASSEMBLY_USAGE_OCCURRENCE ( 'NAUO19', ' ', ' ', #4551, #944, $ ) ;
#8624 = NEXT_ASSEMBLY_USAGE_OCCURRENCE ( 'NAUO20', ' ', ' ', #4551, #4673, $ ) ;
#8625 = NEXT_ASSEMBLY_USAGE_OCCURRENCE ( 'NAUO21', ' ', ' ', #4551, #3008, $ ) ;
#8626 = NEXT_ASSEMBLY_USAGE_OCCURRENCE ( 'NAUO22', ' ', ' ', #4551, #3118, $ ) ;
#8627 = NEXT_ASSEMBLY_USAGE_OCCURRENCE ( 'NAUO23', ' ', ' ', #4551, #7643, $ ) ;
#8628 = NEXT_ASSEMBLY_USAGE_OCCURRENCE ( 'NAUO24', ' ', ' ', #4551, #7017, $ ) ;
#8629 = NEXT_ASSEMBLY_USAGE_OCCURRENCE ( 'NAUO25', ' ', ' ', #4551, #7017, $ ) ;
#8630 = NEXT_ASSEMBLY_USAGE_OCCURRENCE ( 'NAUO26', ' ', ' ', #4551, #7017, $ ) ;
#8631 = NEXT_ASSEMBLY_USAGE_OCCURRENCE ( 'NAUO27', ' ', ' ', #4551, #7017, $ ) ;
#8632 = NEXT_ASSEMBLY_USAGE_OCCURRENCE ( 'NAUO28', ' ', ' ', #4551, #7017, $ ) ;
#8633 = NEXT_ASSEMBLY_USAGE_OCCURRENCE ( 'NAUO29', ' ', ' ', #4551, #7017, $ ) ;
#8634 = NEXT_ASSEMBLY_USAGE_OCCURRENCE ( 'NAUO30', ' ', ' ', #4551, #7017, $ ) ;
#8635 = NEXT_ASSEMBLY_USAGE_OCCURRENCE ( 'NAUO31', ' ', ' ', #4551, #7017, $ ) ;
#8636=COLOUR_RGB('Dark Blue',0.08,0.2,0.34);
#8637=FILL_AREA_STYLE_COLOUR('',#8636);
#8638=FILL_AREA_STYLE('',(#8637));
#8639=SURFACE_STYLE_FILL_AREA(#8638);
#8640=SURFACE_SIDE_STYLE('',(#8639));
#8641=SURFACE_STYLE_USAGE(.BOTH.,#8640);
#8642=PRESENTATION_STYLE_ASSIGNMENT((#8641));
#8643=COLOUR_RGB('Light Blue',0.38,0.62,0.78);
#8644=FILL_AREA_STYLE_COLOUR('',#8643);
#8645=FILL_AREA_STYLE('',(#8644));
#8646=SURFACE_STYLE_FILL_AREA(#8645);
#8647=SURFACE_SIDE_STYLE('',(#8646));
#8648=SURFACE_STYLE_USAGE(.BOTH.,#8647);
#8649=PRESENTATION_STYLE_ASSIGNMENT((#8648));
#8650=COLOUR_RGB('Sky Blue',0.24,0.69,0.87);
#8651=FILL_AREA_STYLE_COLOUR('',#8650);
#8652=FILL_AREA_STYLE('',(#8651));
#8653=SURFACE_STYLE_FILL_AREA(#8652);
#8654=SURFACE_SIDE_STYLE('',(#8653));
#8655=SURFACE_STYLE_USAGE(.BOTH.,#8654);
#8656=PRESENTATION_STYLE_ASSIGNMENT((#8655));
#8657=COLOUR_RGB('Grey',0.48,0.52,0.57);
#8658=FILL_AREA_STYLE_COLOUR('',#8657);
#8659=FILL_AREA_STYLE('',(#8658));
#8660=SURFACE_STYLE_FILL_AREA(#8659);
#8661=SURFACE_SIDE_STYLE('',(#8660));
#8662=SURFACE_STYLE_USAGE(.BOTH.,#8661);
#8663=PRESENTATION_STYLE_ASSIGNMENT((#8662));
#8664=COLOUR_RGB('Black',0.12,0.14,0.17);
#8665=FILL_AREA_STYLE_COLOUR('',#8664);
#8666=FILL_AREA_STYLE('',(#8665));
#8667=SURFACE_STYLE_FILL_AREA(#8666);
#8668=SURFACE_SIDE_STYLE('',(#8667));
#8669=SURFACE_STYLE_USAGE(.BOTH.,#8668);
#8670=PRESENTATION_STYLE_ASSIGNMENT((#8669));
#8671=COLOUR_RGB('Off White',0.89,0.88,0.83);
#8672=FILL_AREA_STYLE_COLOUR('',#8671);
#8673=FILL_AREA_STYLE('',(#8672));
#8674=SURFACE_STYLE_FILL_AREA(#8673);
#8675=SURFACE_SIDE_STYLE('',(#8674));
#8676=SURFACE_STYLE_USAGE(.BOTH.,#8675);
#8677=PRESENTATION_STYLE_ASSIGNMENT((#8676));
ENDSEC;
END-ISO-10303-21;
